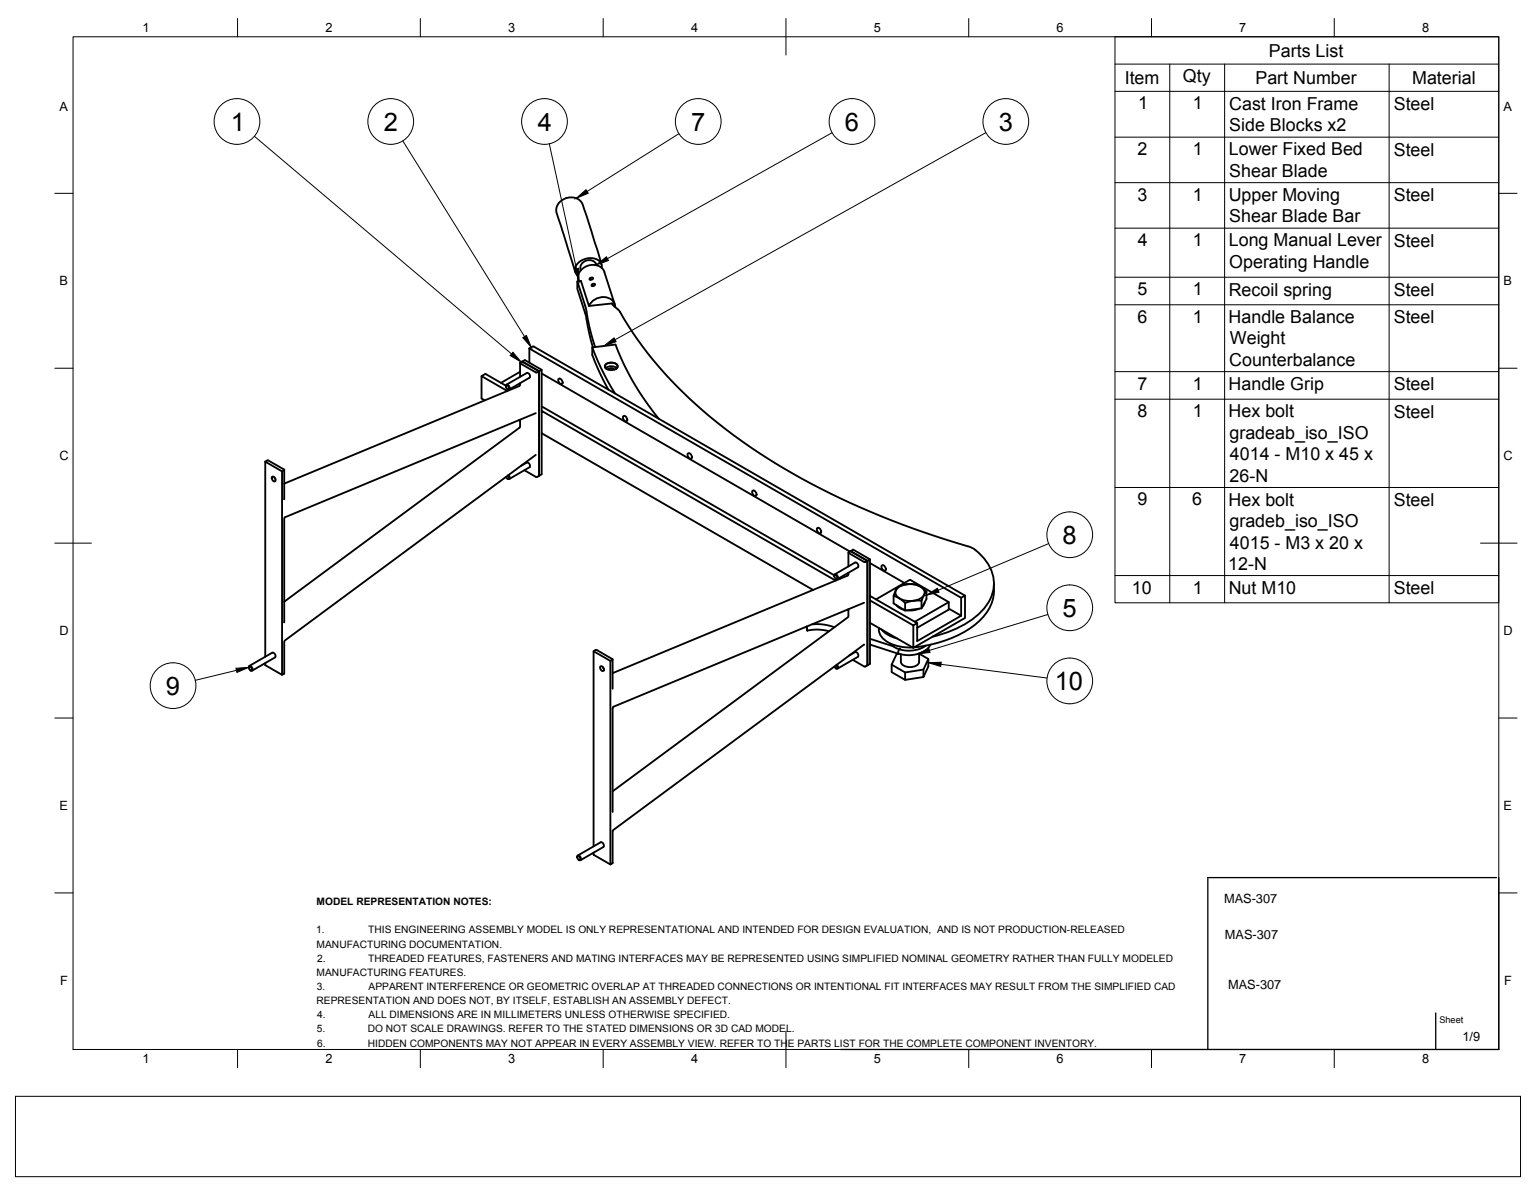
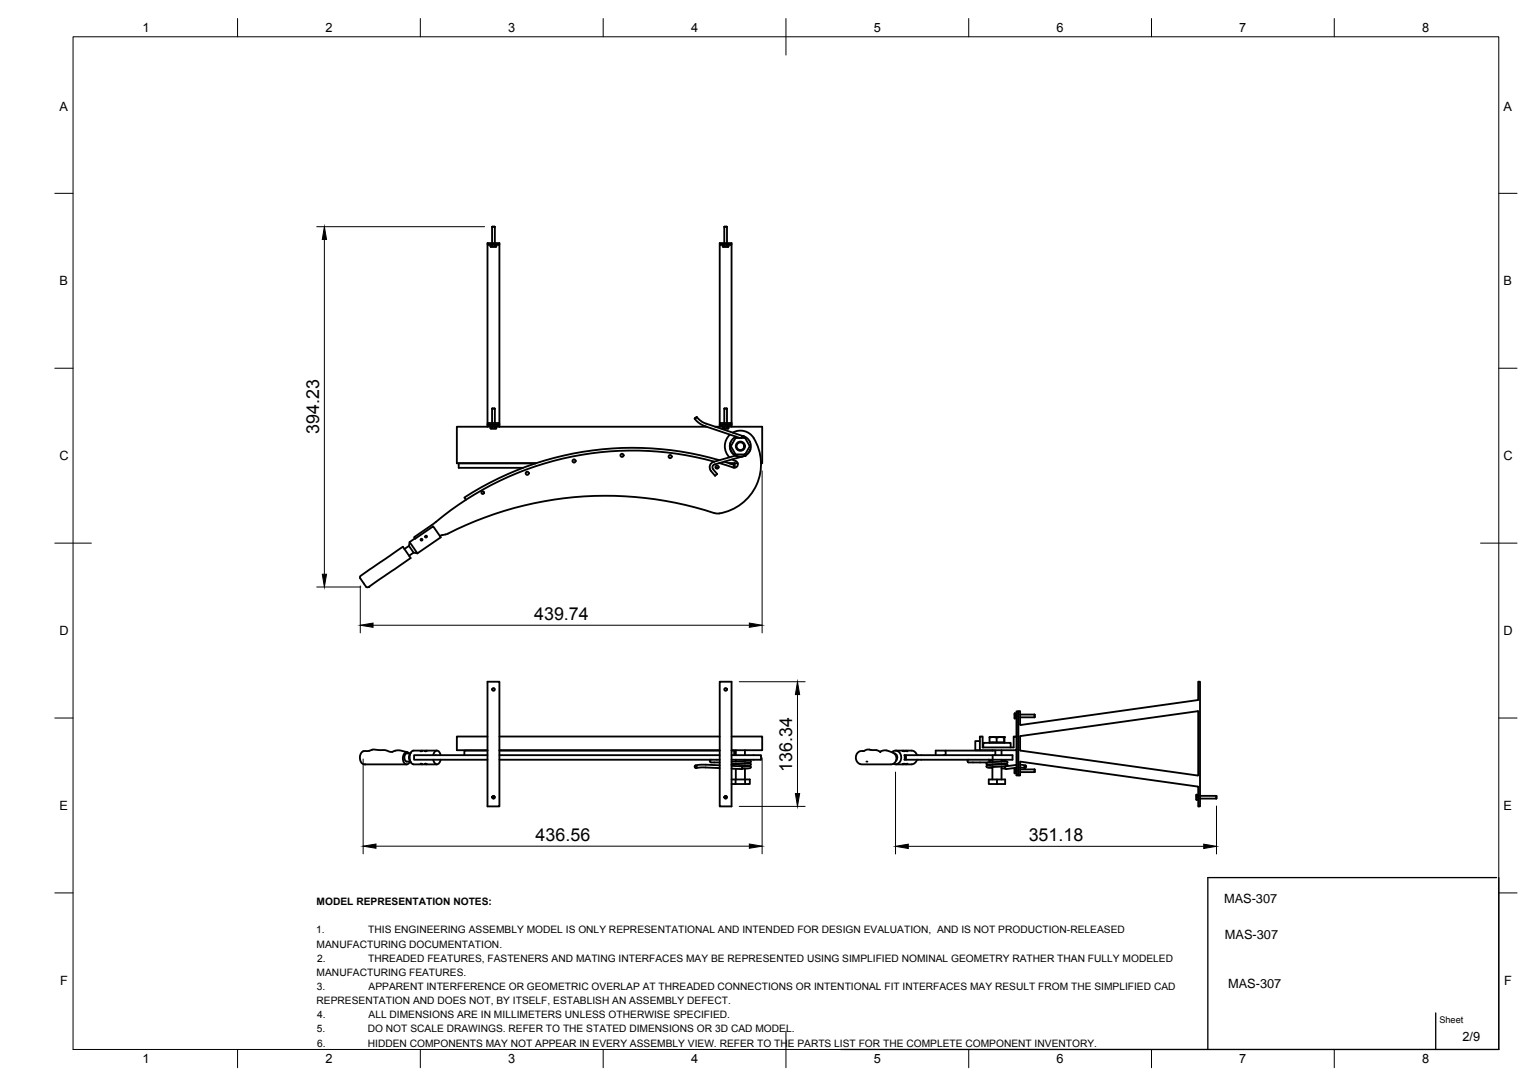
ISO-10303-21;
HEADER;
FILE_DESCRIPTION (('STEP AP214'),
    '1' );
FILE_NAME ('MAS-307',
    '2026-10-06T07:34:29',
    ( '' ),
    ( '' ),
    'SwSTEP 2.0',
    'SolidWorks 2025',
    '' );
FILE_SCHEMA (( 'AUTOMOTIVE_DESIGN' ));
ENDSEC;

DATA;
#1 = ORIENTED_EDGE ( 'NONE', *, *, #36, .T. ) ;
#2 = DIRECTION ( 'NONE',  ( 0.000000000000000000, 0.000000000000000000, -1.000000000000000000 ) ) ;
#3 = CIRCLE ( 'NONE', #12613, 8.000000000000028422 ) ;
#4 = CARTESIAN_POINT ( 'NONE',  ( 177.5000000000000853, 15.47035339324670922, 37.00486596562913633 ) ) ;
#5 = CIRCLE ( 'NONE', #1538, 3.525000000000000355 ) ;
#6 = CARTESIAN_POINT ( 'NONE',  ( -167.5053995445195767, 127.4304153265770907, 2.500000001036336350 ) ) ;
#7 = CARTESIAN_POINT ( 'NONE',  ( -70.00000000000000000, -201.3058001507315566, -41.45141194869120227 ) ) ;
#8 = ORIENTED_EDGE ( 'NONE', *, *, #9613, .T. ) ;
#9 = EDGE_LOOP ( 'NONE', ( #498, #10940, #14960, #5861, #9835 ) ) ;
#10 = CARTESIAN_POINT ( 'NONE',  ( -168.3602667112202766, 125.8948777600411830, -3.002243219525047024 ) ) ;
#11 = CARTESIAN_POINT ( 'NONE',  ( 205.4931693814993139, 33.91842896272902408, -6.501828201457912293 ) ) ;
#12 = ORIENTED_EDGE ( 'NONE', *, *, #8305, .F. ) ;
#13 = DIRECTION ( 'NONE',  ( 0.000000000000000000, 0.1391731009600660485, -0.9902680687415702510 ) ) ;
#14 = LINE ( 'NONE', #12973, #6716 ) ;
#15 = CARTESIAN_POINT ( 'NONE',  ( 66.76535645333922275, 38.79159067395544014, 7.600000000000002309 ) ) ;
#16 = VECTOR ( 'NONE', #3003, 1000.000000000000000 ) ;
#17 = EDGE_CURVE ( 'NONE', #5528, #10245, #15139, .T. ) ;
#18 = MECHANICAL_DESIGN_GEOMETRIC_PRESENTATION_REPRESENTATION (  '', ( #1288 ), #7370 ) ;
#19 = ORIENTED_EDGE ( 'NONE', *, *, #12875, .F. ) ;
#20 = DIRECTION ( 'NONE',  ( -0.000000000000000000, -0.000000000000000000, 1.000000000000000000 ) ) ;
#21 = CARTESIAN_POINT ( 'NONE',  ( 205.4699394944333051, 33.88363592193200446, -7.930995773285529182 ) ) ;
#22 = ORIENTED_EDGE ( 'NONE', *, *, #8785, .F. ) ;
#23 = DIRECTION ( 'NONE',  ( -0.000000000000000000, 1.156482317317871478E-16, -1.000000000000000000 ) ) ;
#24 = CARTESIAN_POINT ( 'NONE',  ( -136.1405586187959784, 108.3975249866138597, 0.000000000000000000 ) ) ;
#25 = CARTESIAN_POINT ( 'NONE',  ( -225.5636091402884915, 143.1065995042388863, -0.5218507872395625746 ) ) ;
#26 = LINE ( 'NONE', #1296, #2230 ) ;
#27 = ORIENTED_EDGE ( 'NONE', *, *, #13841, .F. ) ;
#28 = CARTESIAN_POINT ( 'NONE',  ( -185.2335129678179726, 125.0353967269121966, 9.577123744044223841 ) ) ;
#30 = CARTESIAN_POINT ( 'NONE',  ( 198.8634854004546071, 49.55149448133588663, -6.680369717582868461 ) ) ;
#29 = VECTOR ( 'NONE', #1575, 1000.000000000000000 ) ;
#31 = ORIENTED_EDGE ( 'NONE', *, *, #9479, .F. ) ;
#32 = ORIENTED_EDGE ( 'NONE', *, *, #11983, .F. ) ;
#33 = VECTOR ( 'NONE', #1804, 1000.000000000000000 ) ;
#34 = DIRECTION ( 'NONE',  ( -0.000000000000000000, -0.000000000000000000, 1.000000000000000000 ) ) ;
#35 = LINE ( 'NONE', #4552, #8075 ) ;
#36 = EDGE_CURVE ( 'NONE', #15150, #10379, #8408, .T. ) ;
#37 = DIRECTION ( 'NONE',  ( 0.000000000000000000, 0.000000000000000000, -1.000000000000000000 ) ) ;
#38 = DIRECTION ( 'NONE',  ( 1.000000000000000000, 0.000000000000000000, 0.000000000000000000 ) ) ;
#39 = CARTESIAN_POINT ( 'NONE',  ( -152.4086188282879277, 107.2728346664360259, 84.88378295107887084 ) ) ;
#40 = PRODUCT_RELATED_PRODUCT_CATEGORY ( 'part', '', ( #10548 ) ) ;
#41 = CARTESIAN_POINT ( 'NONE',  ( -150.4086188282879277, 107.2728346664360259, 5.000000000000004441 ) ) ;
#42 = CONICAL_SURFACE ( 'NONE', #4331, 4.499999999999950262, 0.7853981633974450594 ) ;
#43 = DIRECTION ( 'NONE',  ( 0.000000000000000000, 0.000000000000000000, 1.000000000000000000 ) ) ;
#44 = EDGE_CURVE ( 'NONE', #6556, #10266, #3803, .T. ) ;
#45 = CARTESIAN_POINT ( 'NONE',  ( -76.50000000000001421, 15.03993994372673981, 10.05257423913146475 ) ) ;
#46 = FACE_OUTER_BOUND ( 'NONE', #2849, .T. ) ;
#47 = CARTESIAN_POINT ( 'NONE',  ( 70.26535645333922275, 38.79159067395544014, 10.00000000000000178 ) ) ;
#48 = CARTESIAN_POINT ( 'NONE',  ( 177.5000000000000853, 15.03993994372673804, 24.94742576086838781 ) ) ;
#49 = ORIENTED_EDGE ( 'NONE', *, *, #2623, .T. ) ;
#50 = VERTEX_POINT ( 'NONE', #13007 ) ;
#51 = DIRECTION ( 'NONE',  ( 1.000000000000000000, 0.000000000000000000, 0.000000000000000000 ) ) ;
#52 = CARTESIAN_POINT ( 'NONE',  ( -36.49899788034579018, 48.72489408690345414, 5.000000000000000000 ) ) ;
#53 = PLANE ( 'NONE',  #11171 ) ;
#54 = FACE_OUTER_BOUND ( 'NONE', #8334, .T. ) ;
#55 = CARTESIAN_POINT ( 'NONE',  ( -76.50000000000001421, 19.53993994372674692, -17.50000000000002487 ) ) ;
#56 = TOROIDAL_SURFACE ( 'NONE', #1821, 4.799128011492294732, 1.499999999999997113 ) ;
#57 = DIRECTION ( 'NONE',  ( 1.000000000000000000, 0.000000000000000000, 0.000000000000000000 ) ) ;
#58 = FACE_OUTER_BOUND ( 'NONE', #1129, .T. ) ;
#59 = EDGE_CURVE ( 'NONE', #163, #6601, #13932, .T. ) ;
#60 = EDGE_CURVE ( 'NONE', #13786, #6568, #5831, .T. ) ;
#61 = VERTEX_POINT ( 'NONE', #1883 ) ;
#62 = AXIS2_PLACEMENT_3D ( 'NONE', #15140, #11528, #6573 ) ;
#63 = ORIENTED_EDGE ( 'NONE', *, *, #11844, .T. ) ;
#64 = CARTESIAN_POINT ( 'NONE',  ( 207.1592428330643827, 35.64176030267155681, -3.375779224823745928 ) ) ;
#65 = LINE ( 'NONE', #4977, #10142 ) ;
#66 = ORIENTED_EDGE ( 'NONE', *, *, #14903, .T. ) ;
#67 = VECTOR ( 'NONE', #9001, 1000.000000000000000 ) ;
#68 = CARTESIAN_POINT ( 'NONE',  ( -223.5763732829059904, 146.6670444861485976, 6.843617190574383891 ) ) ;
#69 = EDGE_LOOP ( 'NONE', ( #4641, #9788 ) ) ;
#70 = DIRECTION ( 'NONE',  ( -3.965082230804130220E-16, -0.000000000000000000, -1.000000000000000000 ) ) ;
#71 = CARTESIAN_POINT ( 'NONE',  ( 198.4684236769687686, 29.09143143995051872, -2.316743362709667409 ) ) ;
#72 = EDGE_CURVE ( 'NONE', #11235, #14746, #6724, .T. ) ;
#74 = ORIENTED_EDGE ( 'NONE', *, *, #9272, .F. ) ;
#73 = AXIS2_PLACEMENT_3D ( 'NONE', #11589, #11673, #2027 ) ;
#75 = FACE_OUTER_BOUND ( 'NONE', #2731, .T. ) ;
#76 = CARTESIAN_POINT ( 'NONE',  ( 70.26535645333922275, 38.79159067395544014, 7.600000000000002309 ) ) ;
#77 = LINE ( 'NONE', #10922, #4868 ) ;
#78 = VECTOR ( 'NONE', #416, 1000.000000000000000 ) ;
#79 = ORIENTED_EDGE ( 'NONE', *, *, #3059, .T. ) ;
#80 = CIRCLE ( 'NONE', #13699, 3.525000000000000355 ) ;
#81 = CARTESIAN_POINT ( 'NONE',  ( -110.0000000000000426, 59.53993994372674337, 10.00000000000000178 ) ) ;
#82 = DIRECTION ( 'NONE',  ( -0.000000000000000000, -0.000000000000000000, 1.000000000000000000 ) ) ;
#83 = ADVANCED_FACE ( 'NONE', ( #687 ), #5531, .F. ) ;
#84 = DIRECTION ( 'NONE',  ( 1.000000000000000000, 0.000000000000000000, 0.000000000000000000 ) ) ;
#85 = VERTEX_POINT ( 'NONE', #2360 ) ;
#86 = EDGE_LOOP ( 'NONE', ( #3348, #2604, #2165, #14498 ) ) ;
#87 = CARTESIAN_POINT ( 'NONE',  ( -207.0700983879231387, 149.0508413170868209, -0.4547266291960758156 ) ) ;
#88 = CARTESIAN_POINT ( 'NONE',  ( 198.7876695280922661, 49.53587328158837977, -8.249370650301745655 ) ) ;
#89 = ORIENTED_EDGE ( 'NONE', *, *, #715, .T. ) ;
#90 = LINE ( 'NONE', #10937, #11841 ) ;
#91 = FACE_OUTER_BOUND ( 'NONE', #15309, .T. ) ;
#92 = CARTESIAN_POINT ( 'NONE',  ( 178.0000000000000853, 15.03993994372673981, -3.075184203610571654 ) ) ;
#93 = ORIENTED_EDGE ( 'NONE', *, *, #2529, .F. ) ;
#94 = AXIS2_PLACEMENT_3D ( 'NONE', #7418, #12210, #6221 ) ;
#95 = CARTESIAN_POINT ( 'NONE',  ( 201.7406124912899941, 52.65652330452660834, -2.244206067705167396 ) ) ;
#96 = ORIENTED_EDGE ( 'NONE', *, *, #2656, .T. ) ;
#97 = CARTESIAN_POINT ( 'NONE',  ( -34.79899788034579444, 48.72489408690345414, 10.00000000000000178 ) ) ;
#98 = CARTESIAN_POINT ( 'NONE',  ( 175.9483885134608272, -181.3058001507315566, -51.45141194869120227 ) ) ;
#99 = CARTESIAN_POINT ( 'NONE',  ( -218.1518098834511648, 139.2461763302102327, 3.478895870929506362 ) ) ;
#100 = DIRECTION ( 'NONE',  ( -1.000000000000000000, 0.000000000000000000, 0.000000000000000000 ) ) ;
#101 = VERTEX_POINT ( 'NONE', #4890 ) ;
#102 = CARTESIAN_POINT ( 'NONE',  ( -182.6699909761611877, 123.4132960977408970, 9.577123744044220288 ) ) ;
#103 = CARTESIAN_POINT ( 'NONE',  ( 202.3883256910358739, 32.65987148549056229, -8.116337980372584582 ) ) ;
#104 = ORIENTED_EDGE ( 'NONE', *, *, #13012, .T. ) ;
#105 = ORIENTED_EDGE ( 'NONE', *, *, #5952, .T. ) ;
#106 = CYLINDRICAL_SURFACE ( 'NONE', #2526, 3.752352628381527833 ) ;
#107 = LINE ( 'NONE', #4949, #8591 ) ;
#108 = VECTOR ( 'NONE', #10524, 1000.000000000000000 ) ;
#109 = DIRECTION ( 'NONE',  ( -0.000000000000000000, -0.000000000000000000, 1.000000000000000000 ) ) ;
#110 = CARTESIAN_POINT ( 'NONE',  ( 5.799999999999999822, -4.618802153517037823, -7.999999999999979572 ) ) ;
#111 = ADVANCED_FACE ( 'NONE', ( #1394 ), #10899, .F. ) ;
#112 = CARTESIAN_POINT ( 'NONE',  ( -225.3482675701515348, 143.4924177300907502, -0.7821592797845021705 ) ) ;
#113 = DIRECTION ( 'NONE',  ( 1.000000000000000000, 0.000000000000000000, 0.000000000000000000 ) ) ;
#114 = CARTESIAN_POINT ( 'NONE',  ( -35.99999999999995026, 62.13993994372673768, 18.50000000000140332 ) ) ;
#115 = AXIS2_PLACEMENT_3D ( 'NONE', #5696, #3243, #10590 ) ;
#116 = CARTESIAN_POINT ( 'NONE',  ( -108.0000000000000568, 64.53993994372673626, 20.00000000000000355 ) ) ;
#117 = DIRECTION ( 'NONE',  ( 0.000000000000000000, 0.000000000000000000, 1.000000000000000000 ) ) ;
#118 = ORIENTED_EDGE ( 'NONE', *, *, #6762, .T. ) ;
#119 = CARTESIAN_POINT ( 'NONE',  ( 114.0000000000000568, 64.53993994372673626, 11.50000000000034817 ) ) ;
#120 = ADVANCED_FACE ( 'NONE', ( #7198 ), #13161, .F. ) ;
#121 = ORIENTED_EDGE ( 'NONE', *, *, #6164, .F. ) ;
#122 = DIRECTION ( 'NONE',  ( 1.000000000000000000, 0.000000000000000000, 0.000000000000000000 ) ) ;
#123 = DIRECTION ( 'NONE',  ( -0.9741547192086867923, 0.2258817899775114602, 0.000000000000000000 ) ) ;
#124 = FACE_OUTER_BOUND ( 'NONE', #1519, .T. ) ;
#125 = LINE ( 'NONE', #13401, #6173 ) ;
#126 = CARTESIAN_POINT ( 'NONE',  ( 185.1062858801516882, 25.86394065090268057, 18.00000000000000355 ) ) ;
#127 = CARTESIAN_POINT ( 'NONE',  ( 0.000000000000000000, -2.381569860407207084, -1.374999999999997113 ) ) ;
#128 = DIRECTION ( 'NONE',  ( 0.000000000000000000, 0.000000000000000000, -1.000000000000000000 ) ) ;
#129 = AXIS2_PLACEMENT_3D ( 'NONE', #758, #2991, #9229 ) ;
#130 = EDGE_LOOP ( 'NONE', ( #9688, #11393, #15136, #3970 ) ) ;
#131 = ORIENTED_EDGE ( 'NONE', *, *, #13724, .F. ) ;
#132 = CARTESIAN_POINT ( 'NONE',  ( 202.9578473199472057, 32.84482942423175444, -9.656098271102047548 ) ) ;
#133 = CARTESIAN_POINT ( 'NONE',  ( -221.9693044472552117, 149.5463605724702916, 7.947916423171728084 ) ) ;
#134 = ORIENTED_EDGE ( 'NONE', *, *, #1310, .F. ) ;
#135 = ADVANCED_FACE ( 'NONE', ( #124, #11996 ), #53, .F. ) ;
#136 = CARTESIAN_POINT ( 'NONE',  ( -222.7380986314676363, 148.1689451111236906, 7.733218891984481758 ) ) ;
#137 = EDGE_CURVE ( 'NONE', #9526, #14472, #1038, .T. ) ;
#138 = VERTEX_POINT ( 'NONE', #10733 ) ;
#139 = CARTESIAN_POINT ( 'NONE',  ( 164.0000000000000568, 64.53993994372673626, 16.70000000000000995 ) ) ;
#140 = AXIS2_PLACEMENT_3D ( 'NONE', #4727, #9874, #2603 ) ;
#141 = CARTESIAN_POINT ( 'NONE',  ( 177.5000000000000853, -179.3058001507315566, -51.45141194869120227 ) ) ;
#142 = CIRCLE ( 'NONE', #13010, 4.499999999999950262 ) ;
#143 = ORIENTED_EDGE ( 'NONE', *, *, #13656, .T. ) ;
#144 = CARTESIAN_POINT ( 'NONE',  ( 114.0000000000000426, 15.53993994372673981, 7.305634244248866343E-16 ) ) ;
#145 = DIRECTION ( 'NONE',  ( -5.518327896226365911E-17, 0.9902680687415714722, -0.1391731009600582769 ) ) ;
#146 = B_SPLINE_CURVE_WITH_KNOTS ( 'NONE', 3,
 ( #5136, #531, #1653, #11218, #9963, #14979, #8698, #12464, #14906, #1729, #5371, #4019, #13643, #371, #7438, #2772, #5212, #6490, #11287, #14749, #7674, #6569, #448, #13727, #10034, #10112, #10189, #12233, #8933, #1411, #2930, #11372, #4170, #6248, #1492, #211, #11061, #2692, #5059, #9884, #14674, #3874, #685, #1881, #15369, #849, #13889, #9240 ),
 .UNSPECIFIED., .F., .F.,
 ( 4, 2, 2, 2, 2, 2, 2, 2, 2, 2, 2, 2, 2, 2, 2, 2, 2, 2, 2, 2, 2, 2, 2, 4 ),
 ( 0.02192817935270313656, 0.02330785662426448565, 0.02399769526004516540, 0.02468753389582584862, 0.02606721116738722893, 0.02675704980316793297, 0.02744688843894863700, 0.02882656571051007630, 0.02951640434629079768, 0.03020624298207151559, 0.03158592025363299305, 0.03227575888941371096, 0.03296559752519442887, 0.03365543616097514679, 0.03434527479675586470, 0.03572495206831733522, 0.03641479070409808783, 0.03710462933987884043, 0.03779446797565959304, 0.03848430661144034565, 0.03986398388300183004, 0.04124366115456330750, 0.04262333842612478496, 0.04400301569768626936 ),
 .UNSPECIFIED. ) ;
#147 = PLANE ( 'NONE',  #811 ) ;
#148 = EDGE_LOOP ( 'NONE', ( #966, #9881, #15338, #13043 ) ) ;
#149 = ORIENTED_EDGE ( 'NONE', *, *, #15360, .T. ) ;
#150 = CARTESIAN_POINT ( 'NONE',  ( 190.5000000000000568, -181.3058001507315566, 84.88378295107885663 ) ) ;
#151 = ORIENTED_EDGE ( 'NONE', *, *, #11944, .F. ) ;
#152 = FACE_OUTER_BOUND ( 'NONE', #9575, .T. ) ;
#153 = CARTESIAN_POINT ( 'NONE',  ( -152.0435700508773209, 108.0561044943065951, -4.829560219627783368 ) ) ;
#154 = ORIENTED_EDGE ( 'NONE', *, *, #12875, .T. ) ;
#155 = ORIENTED_EDGE ( 'NONE', *, *, #7793, .T. ) ;
#156 = CARTESIAN_POINT ( 'NONE',  ( -179.9223906590855222, 134.3711564447467310, 1.515441477536284554 ) ) ;
#157 = CARTESIAN_POINT ( 'NONE',  ( -223.6137413416247739, 142.0138547493179146, 2.263321283727593336 ) ) ;
#158 = VERTEX_POINT ( 'NONE', #7269 ) ;
#159 = CIRCLE ( 'NONE', #9018, 4.499999999999950262 ) ;
#160 = DIRECTION ( 'NONE',  ( 0.000000000000000000, 0.9902680687415712502, 0.1391731009600584990 ) ) ;
#161 = DIRECTION ( 'NONE',  ( 0.000000000000000000, 0.000000000000000000, -1.000000000000000000 ) ) ;
#162 = DIRECTION ( 'NONE',  ( 8.659560562354932858E-17, 0.7071067811865474617, -0.7071067811865474617 ) ) ;
#163 = VERTEX_POINT ( 'NONE', #8301 ) ;
#164 = EDGE_CURVE ( 'NONE', #1358, #7203, #12629, .T. ) ;
#165 = LINE ( 'NONE', #5013, #3777 ) ;
#166 = CARTESIAN_POINT ( 'NONE',  ( 198.3913412372077687, 29.09831693401786268, -0.7477385443502184703 ) ) ;
#167 = ORIENTED_EDGE ( 'NONE', *, *, #13377, .T. ) ;
#168 = CARTESIAN_POINT ( 'NONE',  ( -64.00000000000002842, 15.53993994372673981, -3.075184203610571654 ) ) ;
#169 = AXIS2_PLACEMENT_3D ( 'NONE', #9896, #5224, #1587 ) ;
#170 = CARTESIAN_POINT ( 'NONE',  ( -183.7136537759689929, 127.7093858820786068, -5.230826428279597096 ) ) ;
#171 = CARTESIAN_POINT ( 'NONE',  ( -63.50000000000002842, 15.03993994372673981, -3.075184203610571654 ) ) ;
#172 = ORIENTED_EDGE ( 'NONE', *, *, #9722, .T. ) ;
#173 = CARTESIAN_POINT ( 'NONE',  ( -197.4591130885309553, 135.0981391493542105, 10.16010209732750802 ) ) ;
#174 = CARTESIAN_POINT ( 'NONE',  ( 207.1690005588685040, 46.08364065960329725, 0.3832845883476674320 ) ) ;
#175 = ORIENTED_EDGE ( 'NONE', *, *, #1719, .F. ) ;
#176 = VERTEX_POINT ( 'NONE', #14424 ) ;
#177 = AXIS2_PLACEMENT_3D ( 'NONE', #9070, #13874, #12756 ) ;
#178 = CARTESIAN_POINT ( 'NONE',  ( -85.99999999999994316, 64.51493994372674479, 18.50000000000175149 ) ) ;
#179 = DIRECTION ( 'NONE',  ( 0.000000000000000000, 0.000000000000000000, 1.000000000000000000 ) ) ;
#180 =( GEOMETRIC_REPRESENTATION_CONTEXT ( 3 ) GLOBAL_UNCERTAINTY_ASSIGNED_CONTEXT ( ( #8186 ) ) GLOBAL_UNIT_ASSIGNED_CONTEXT ( ( #3150, #4481, #1954 ) ) REPRESENTATION_CONTEXT ( 'NONE', 'WORKASPACE' ) );
#181 = CARTESIAN_POINT ( 'NONE',  ( 200.1062858801516597, 40.86394065090267702, 12.00000000000001066 ) ) ;
#182 = TOROIDAL_SURFACE ( 'NONE', #1206, 1.000000000000000000, 0.5000000000000000000 ) ;
#183 = DIRECTION ( 'NONE',  ( 1.000000000000000000, 0.000000000000000000, 0.000000000000000000 ) ) ;
#184 = DIRECTION ( 'NONE',  ( -0.000000000000000000, -0.000000000000000000, 1.000000000000000000 ) ) ;
#185 = AXIS2_PLACEMENT_3D ( 'NONE', #1249, #10903, #14351 ) ;
#186 = DIRECTION ( 'NONE',  ( 0.000000000000000000, 0.000000000000000000, 1.000000000000000000 ) ) ;
#187 = DIRECTION ( 'NONE',  ( 0.000000000000000000, 0.000000000000000000, 1.000000000000000000 ) ) ;
#188 = PRODUCT_DEFINITION_FORMATION_WITH_SPECIFIED_SOURCE ( 'ANY', '', #10425, .NOT_KNOWN. ) ;
#189 = ORIENTED_EDGE ( 'NONE', *, *, #8600, .F. ) ;
#190 = ADVANCED_FACE ( 'NONE', ( #12144 ), #4855, .T. ) ;
#191 = AXIS2_PLACEMENT_3D ( 'NONE', #8581, #13373, #8730 ) ;
#192 = ORIENTED_EDGE ( 'NONE', *, *, #11037, .F. ) ;
#193 = DIRECTION ( 'NONE',  ( 0.000000000000000000, 0.000000000000000000, -1.000000000000000000 ) ) ;
#194 = LINE ( 'NONE', #8457, #6371 ) ;
#195 = DIRECTION ( 'NONE',  ( 1.000000000000000000, 0.000000000000000000, -0.000000000000000000 ) ) ;
#196 = DIRECTION ( 'NONE',  ( 0.000000000000000000, 0.000000000000000000, 1.000000000000000000 ) ) ;
#197 = DIRECTION ( 'NONE',  ( 1.000000000000000000, 0.000000000000000000, 0.000000000000000000 ) ) ;
#198 = DIRECTION ( 'NONE',  ( 0.000000000000000000, 0.000000000000000000, 1.000000000000000000 ) ) ;
#199 = CARTESIAN_POINT ( 'NONE',  ( -185.2055264765504887, 137.3096093875189467, 2.500000000000000000 ) ) ;
#200 = VECTOR ( 'NONE', #3620, 1000.000000000000000 ) ;
#201 = EDGE_LOOP ( 'NONE', ( #1693, #11095, #14591, #7867 ) ) ;
#202 = AXIS2_PLACEMENT_3D ( 'NONE', #6427, #5227, #1671 ) ;
#203 = EDGE_CURVE ( 'NONE', #12014, #13507, #9648, .T. ) ;
#204 = DIRECTION ( 'NONE',  ( 1.000000000000000000, 0.000000000000000000, 0.000000000000000000 ) ) ;
#205 = CARTESIAN_POINT ( 'NONE',  ( 205.4339596421060889, 33.86846485884471747, -4.932823326473320336 ) ) ;
#206 = CARTESIAN_POINT ( 'NONE',  ( -224.5476011597490356, 144.9269372877251669, 3.604463283145519448 ) ) ;
#207 = VERTEX_POINT ( 'NONE', #5995 ) ;
#208 = CIRCLE ( 'NONE', #2252, 1.499999999999996891 ) ;
#209 = CARTESIAN_POINT ( 'NONE',  ( -222.3356595723642215, 144.5667354790973604, 8.419022500423421818 ) ) ;
#210 = EDGE_LOOP ( 'NONE', ( #10445, #12034, #11284, #6545 ) ) ;
#211 = CARTESIAN_POINT ( 'NONE',  ( -172.9645346626803359, 118.3395572346633173, -3.768257758897336274 ) ) ;
#212 = CARTESIAN_POINT ( 'NONE',  ( 192.9105869384611935, 31.39693960586098598, -5.567602151433582058 ) ) ;
#213 = CIRCLE ( 'NONE', #730, 1.000000000000000888 ) ;
#214 = VECTOR ( 'NONE', #12787, 1000.000000000000227 ) ;
#215 = ORIENTED_EDGE ( 'NONE', *, *, #12661, .T. ) ;
#216 = CARTESIAN_POINT ( 'NONE',  ( -61.94838851346079167, -178.8058001507315566, 52.69066787724494816 ) ) ;
#217 = CARTESIAN_POINT ( 'NONE',  ( -76.00000000000001421, 15.53993994372674159, 9.617930870223352358 ) ) ;
#218 = EDGE_CURVE ( 'NONE', #11968, #7924, #4346, .T. ) ;
#219 = AXIS2_PLACEMENT_3D ( 'NONE', #7961, #12749, #6770 ) ;
#220 = DIRECTION ( 'NONE',  ( -0.000000000000000000, 1.486905836551548832E-16, -1.000000000000000000 ) ) ;
#221 = ORIENTED_EDGE ( 'NONE', *, *, #12224, .F. ) ;
#222 =( GEOMETRIC_REPRESENTATION_CONTEXT ( 3 ) GLOBAL_UNCERTAINTY_ASSIGNED_CONTEXT ( ( #10529 ) ) GLOBAL_UNIT_ASSIGNED_CONTEXT ( ( #15547, #7222, #9271 ) ) REPRESENTATION_CONTEXT ( 'NONE', 'WORKASPACE' ) );
#223 = AXIS2_PLACEMENT_3D ( 'NONE', #7936, #9115, #2067 ) ;
#224 = PRODUCT_RELATED_PRODUCT_CATEGORY ( 'part', '', ( #9174 ) ) ;
#225 = EDGE_CURVE ( 'NONE', #176, #7789, #1243, .T. ) ;
#226 = DIRECTION ( 'NONE',  ( 1.156482317317871725E-16, 1.156482317317871725E-16, -1.000000000000000000 ) ) ;
#227 = VERTEX_POINT ( 'NONE', #12067 ) ;
#228 = LINE ( 'NONE', #150, #2384 ) ;
#229 = EDGE_CURVE ( 'NONE', #11059, #5257, #8156, .T. ) ;
#230 = EDGE_LOOP ( 'NONE', ( #7966, #6489 ) ) ;
#231 = DIRECTION ( 'NONE',  ( 0.9296197478520974444, 0.3660421972118351741, -0.04266420354037655377 ) ) ;
#232 = DIRECTION ( 'NONE',  ( -0.000000000000000000, 1.000000000000000000, 1.156482317317871725E-16 ) ) ;
#233 = AXIS2_PLACEMENT_3D ( 'NONE', #7331, #6137, #10957 ) ;
#234 = VERTEX_POINT ( 'NONE', #13400 ) ;
#235 = VERTEX_POINT ( 'NONE', #8458 ) ;
#236 = LINE ( 'NONE', #6353, #3489 ) ;
#237 = CARTESIAN_POINT ( 'NONE',  ( 207.1194509196011495, 46.14302886020001182, -1.185720282267065828 ) ) ;
#238 = VECTOR ( 'NONE', #1875, 1000.000000000000000 ) ;
#239 = ORIENTED_EDGE ( 'NONE', *, *, #3705, .T. ) ;
#240 = DIRECTION ( 'NONE',  ( 0.000000000000000000, -1.000000000000000000, 0.000000000000000000 ) ) ;
#241 = CARTESIAN_POINT ( 'NONE',  ( 190.0000000000000568, -179.3058001507315282, -29.88378295107906268 ) ) ;
#242 = FACE_OUTER_BOUND ( 'NONE', #9642, .T. ) ;
#243 = MANIFOLD_SOLID_BREP ( 'HeadFillet', #9878 ) ;
#244 = EDGE_CURVE ( 'NONE', #1879, #4614, #5269, .T. ) ;
#245 = EDGE_CURVE ( 'NONE', #3324, #6496, #6158, .T. ) ;
#246 = AXIS2_PLACEMENT_3D ( 'NONE', #10758, #10919, #3716 ) ;
#247 = CIRCLE ( 'NONE', #14631, 0.5000000000000069944 ) ;
#248 =( LENGTH_UNIT ( ) NAMED_UNIT ( * ) SI_UNIT ( .MILLI., .METRE. ) );
#249 = CARTESIAN_POINT ( 'NONE',  ( 194.7047954745769687, 33.92018974228710704, -0.9908858387024377379 ) ) ;
#250 = ORIENTED_EDGE ( 'NONE', *, *, #12118, .T. ) ;
#251 = DIRECTION ( 'NONE',  ( 0.000000000000000000, 6.938893903907227145E-17, -1.000000000000000000 ) ) ;
#252 = CYLINDRICAL_SURFACE ( 'NONE', #13481, 1.700000000000007061 ) ;
#253 = EDGE_CURVE ( 'NONE', #2275, #9404, #10915, .T. ) ;
#254 = CARTESIAN_POINT ( 'NONE',  ( -176.4863952559862526, 117.0241230567913959, -0.6469977504890583875 ) ) ;
#255 = DIRECTION ( 'NONE',  ( -0.000000000000000000, -0.000000000000000000, 1.000000000000000000 ) ) ;
#256 = VERTEX_POINT ( 'NONE', #7495 ) ;
#257 = CARTESIAN_POINT ( 'NONE',  ( -171.9895241055258168, 125.0924944214600885, 9.516496325551347724 ) ) ;
#258 = CARTESIAN_POINT ( 'NONE',  ( 202.9147226314038051, 48.88641379461363101, -0.9068510277452211943 ) ) ;
#259 = VERTEX_POINT ( 'NONE', #512 ) ;
#260 = EDGE_LOOP ( 'NONE', ( #8120, #14477, #13087, #8621 ) ) ;
#261 = VECTOR ( 'NONE', #6975, 1000.000000000000000 ) ;
#262 = ADVANCED_FACE ( 'NONE', ( #11203, #355 ), #1639, .F. ) ;
#263 = CARTESIAN_POINT ( 'NONE',  ( 14.00000000000004086, 64.53993994372673626, 15.00000000000104983 ) ) ;
#264 = CARTESIAN_POINT ( 'NONE',  ( 0.000000000000000000, 17.53993994372673981, 8.693413025030312018E-16 ) ) ;
#265 = AXIS2_PLACEMENT_3D ( 'NONE', #2568, #9839, #9679 ) ;
#266 = DIRECTION ( 'NONE',  ( -0.000000000000000000, -0.000000000000000000, 1.000000000000000000 ) ) ;
#267 = DIRECTION ( 'NONE',  ( 0.000000000000000000, -1.000000000000000000, -1.156482317317871478E-16 ) ) ;
#268 = AXIS2_PLACEMENT_3D ( 'NONE', #5608, #7835, #11451 ) ;
#269 = MANIFOLD_SOLID_BREP ( 'Move Face1', #9158 ) ;
#270 = LINE ( 'NONE', #1701, #14484 ) ;
#271 = CARTESIAN_POINT ( 'NONE',  ( -218.6464950597879238, 155.4996951832063701, 5.432615396193927637 ) ) ;
#272 = CARTESIAN_POINT ( 'NONE',  ( 14.00000000000004086, 62.13993994372673768, 15.00000000000104983 ) ) ;
#273 = VECTOR ( 'NONE', #10509, 1000.000000000000000 ) ;
#274 = FACE_BOUND ( 'NONE', #5485, .T. ) ;
#275 = ORIENTED_EDGE ( 'NONE', *, *, #10508, .T. ) ;
#276 = CARTESIAN_POINT ( 'NONE',  ( 215.1062858801516882, 55.86394065090267702, 13.00000000000000178 ) ) ;
#277 = ORIENTED_EDGE ( 'NONE', *, *, #6163, .F. ) ;
#278 = EDGE_CURVE ( 'NONE', #319, #8130, #1801, .T. ) ;
#279 = ORIENTED_EDGE ( 'NONE', *, *, #13409, .F. ) ;
#280 = DIRECTION ( 'NONE',  ( 0.000000000000000000, 0.000000000000000000, 1.000000000000000000 ) ) ;
#281 = DIRECTION ( 'NONE',  ( -0.9741547192086869034, 0.2258817899775114879, 0.000000000000000000 ) ) ;
#282 = CARTESIAN_POINT ( 'NONE',  ( 0.7145311798163189732, 4.618802153516981868, 8.000000000000007105 ) ) ;
#283 = CARTESIAN_POINT ( 'NONE',  ( -64.00000000000002842, -179.3058001507315566, 52.76585208085545275 ) ) ;
#284 = CARTESIAN_POINT ( 'NONE',  ( 71.96535645333923981, 38.79159067395544014, 0.000000000000000000 ) ) ;
#285 = DIRECTION ( 'NONE',  ( 1.000000000000000000, -2.751328491981765035E-32, 3.965082230804130220E-16 ) ) ;
#286 = AXIS2_PLACEMENT_3D ( 'NONE', #9137, #2973, #11498 ) ;
#287 = FACE_OUTER_BOUND ( 'NONE', #14918, .T. ) ;
#288 = CARTESIAN_POINT ( 'NONE',  ( -167.5097532647548633, 127.4226149533560175, 3.478855110549762042 ) ) ;
#289 = AXIS2_PLACEMENT_3D ( 'NONE', #7420, #5036, #8676 ) ;
#290 = ORIENTED_EDGE ( 'NONE', *, *, #8264, .F. ) ;
#291 = CARTESIAN_POINT ( 'NONE',  ( 191.3844089520862894, 42.02011290432638901, -3.056456915890917170 ) ) ;
#292 = CARTESIAN_POINT ( 'NONE',  ( -221.1247960154559280, 151.0594299935001743, 7.622044586438916802 ) ) ;
#293 = ORIENTED_EDGE ( 'NONE', *, *, #8057, .F. ) ;
#294 = CARTESIAN_POINT ( 'NONE',  ( -220.5689849208904150, 152.0552528170083519, 9.261189829759533865 ) ) ;
#295 = VERTEX_POINT ( 'NONE', #2676 ) ;
#296 = LINE ( 'NONE', #14821, #5534 ) ;
#297 = VECTOR ( 'NONE', #7988, 1000.000000000000000 ) ;
#298 = CARTESIAN_POINT ( 'NONE',  ( 204.3096479244403554, 51.57035008254927533, -0.9325724660367167296 ) ) ;
#299 = VERTEX_POINT ( 'NONE', #8683 ) ;
#300 = DIRECTION ( 'NONE',  ( 0.000000000000000000, 1.000000000000000000, 0.000000000000000000 ) ) ;
#301 = DIRECTION ( 'NONE',  ( -0.000000000000000000, 6.938893903907222067E-15, -1.000000000000000000 ) ) ;
#302 = DIRECTION ( 'NONE',  ( 1.000000000000000000, 0.000000000000000000, 0.000000000000000000 ) ) ;
#303 = ORIENTED_EDGE ( 'NONE', *, *, #14000, .F. ) ;
#304 = B_SPLINE_CURVE_WITH_KNOTS ( 'NONE', 3,
 ( #12178, #157, #5002, #3249, #8007 ),
 .UNSPECIFIED., .F., .F.,
 ( 4, 1, 4 ),
 ( 2.671544684753287039E-05, 0.0004182544953931666577, 0.0008097935439387997673 ),
 .UNSPECIFIED. ) ;
#305 = APPLICATION_PROTOCOL_DEFINITION ( 'draft international standard', 'automotive_design', 1998, #4533 ) ;
#306 = ORIENTED_EDGE ( 'NONE', *, *, #7823, .F. ) ;
#307 =( NAMED_UNIT ( * ) SI_UNIT ( $, .STERADIAN. ) SOLID_ANGLE_UNIT ( ) );
#308 = CARTESIAN_POINT ( 'NONE',  ( 177.5000000000000853, 17.53993994372673271, 52.49999999999997868 ) ) ;
#309 = EDGE_LOOP ( 'NONE', ( #6645, #5526, #11534, #9026 ) ) ;
#310 = EDGE_CURVE ( 'NONE', #12060, #3478, #2754, .T. ) ;
#311 = CARTESIAN_POINT ( 'NONE',  ( 21.99999999999999289, 0.000000000000000000, 1.219500000000000028 ) ) ;
#312 = COLOUR_RGB ( '', 0.08235294, 0.09019608, 0.10196078) ;
#313 = CARTESIAN_POINT ( 'NONE',  ( 178.0000000000000853, -179.3058001507315566, 84.88378295107887084 ) ) ;
#314 = ORIENTED_EDGE ( 'NONE', *, *, #44, .F. ) ;
#315 = ORIENTED_EDGE ( 'NONE', *, *, #1829, .T. ) ;
#316 = CARTESIAN_POINT ( 'NONE',  ( -214.8715905313398480, 153.8675021612092451, 2.500000000000000000 ) ) ;
#317 = CARTESIAN_POINT ( 'NONE',  ( 207.1167095084715868, 46.15093117762712893, -7.185265714380067337 ) ) ;
#318 = EDGE_CURVE ( 'NONE', #326, #5664, #13476, .T. ) ;
#319 = VERTEX_POINT ( 'NONE', #10023 ) ;
#320 = AXIS2_PLACEMENT_3D ( 'NONE', #10803, #2269, #8291 ) ;
#321 = FACE_BOUND ( 'NONE', #9577, .T. ) ;
#322 = CARTESIAN_POINT ( 'NONE',  ( -64.00000000000002842, -178.8058001507315566, -17.19066787724516843 ) ) ;
#323 = CARTESIAN_POINT ( 'NONE',  ( 184.0000000000000568, -179.3058001507315566, 76.45141194869098911 ) ) ;
#324 = FACE_OUTER_BOUND ( 'NONE', #11938, .T. ) ;
#325 = CARTESIAN_POINT ( 'NONE',  ( 203.1202131991386182, 29.73909689272393564, -6.555651296533415717 ) ) ;
#326 = VERTEX_POINT ( 'NONE', #14806 ) ;
#327 = DIRECTION ( 'NONE',  ( -0.000000000000000000, 1.000000000000000000, 0.000000000000000000 ) ) ;
#328 = CARTESIAN_POINT ( 'NONE',  ( -223.3178949021943538, 142.5860305806809833, -0.6404123112780930605 ) ) ;
#329 = TOROIDAL_SURFACE ( 'NONE', #6419, 4.799128011492294732, 1.499999999999997113 ) ;
#330 = CARTESIAN_POINT ( 'NONE',  ( -207.1238489746795608, 137.1336079999123854, -4.642206099735007641 ) ) ;
#331 = DIRECTION ( 'NONE',  ( 0.000000000000000000, -0.1391731009600591096, 0.9902680687415711391 ) ) ;
#332 = EDGE_LOOP ( 'NONE', ( #12624, #8209, #7735, #9718 ) ) ;
#333 = CARTESIAN_POINT ( 'NONE',  ( -199.4124801547868913, 127.6177204676982910, 1.515400478619089109 ) ) ;
#334 = CARTESIAN_POINT ( 'NONE',  ( 198.9393012728169765, 49.56711568108339350, -5.111368784863990378 ) ) ;
#335 = EDGE_CURVE ( 'NONE', #2939, #10298, #8373, .T. ) ;
#336 = AXIS2_PLACEMENT_3D ( 'NONE', #14411, #13144, #5897 ) ;
#337 = ORIENTED_EDGE ( 'NONE', *, *, #9909, .T. ) ;
#338 = EDGE_CURVE ( 'NONE', #908, #14204, #13896, .T. ) ;
#339 = ORIENTED_EDGE ( 'NONE', *, *, #2372, .F. ) ;
#340 = DIRECTION ( 'NONE',  ( -0.000000000000000000, 1.000000000000000000, -0.000000000000000000 ) ) ;
#341 = CYLINDRICAL_SURFACE ( 'NONE', #1669, 0.5000000000000004441 ) ;
#342 = FACE_OUTER_BOUND ( 'NONE', #1259, .T. ) ;
#343 = MECHANICAL_DESIGN_GEOMETRIC_PRESENTATION_REPRESENTATION (  '', ( #14469 ), #13976 ) ;
#344 = CARTESIAN_POINT ( 'NONE',  ( 70.26535645333922275, 38.79159067395544014, 5.000000000000000000 ) ) ;
#345 = CARTESIAN_POINT ( 'NONE',  ( 190.0000000000001137, -179.3058001507315566, 84.88378295107887084 ) ) ;
#346 = EDGE_CURVE ( 'NONE', #13457, #11923, #1210, .T. ) ;
#347 = CARTESIAN_POINT ( 'NONE',  ( -76.50000000000001421, 15.53993994372673981, -17.50000000000002487 ) ) ;
#348 = DIRECTION ( 'NONE',  ( 0.000000000000000000, 0.000000000000000000, 1.000000000000000000 ) ) ;
#349 = ORIENTED_EDGE ( 'NONE', *, *, #4874, .F. ) ;
#350 = CARTESIAN_POINT ( 'NONE',  ( -70.00000000000000000, 19.53993994372674337, -12.49999999999999467 ) ) ;
#351 = ORIENTED_EDGE ( 'NONE', *, *, #9722, .F. ) ;
#352 = EDGE_LOOP ( 'NONE', ( #9480, #1820, #544, #3677 ) ) ;
#353 = FACE_OUTER_BOUND ( 'NONE', #13566, .T. ) ;
#354 = DIRECTION ( 'NONE',  ( -0.000000000000000000, -0.000000000000000000, 1.000000000000000000 ) ) ;
#355 = FACE_OUTER_BOUND ( 'NONE', #6775, .T. ) ;
#356 = LINE ( 'NONE', #15042, #7156 ) ;
#357 = CYLINDRICAL_SURFACE ( 'NONE', #6736, 1.700000000000001954 ) ;
#358 = CARTESIAN_POINT ( 'NONE',  ( -218.4414990732828699, 155.8669776719573861, 2.805362964459314323 ) ) ;
#359 = CARTESIAN_POINT ( 'NONE',  ( -218.6464950597879238, 155.4996951832063701, 5.432615396193927637 ) ) ;
#360 = ORIENTED_EDGE ( 'NONE', *, *, #11900, .T. ) ;
#361 = AXIS2_PLACEMENT_3D ( 'NONE', #5638, #4281, #10375 ) ;
#362 = EDGE_CURVE ( 'NONE', #3997, #6369, #2486, .T. ) ;
#363 = FACE_OUTER_BOUND ( 'NONE', #2322, .T. ) ;
#364 = EDGE_CURVE ( 'NONE', #10667, #14434, #6613, .T. ) ;
#365 = ADVANCED_FACE ( 'NONE', ( #3595 ), #14635, .F. ) ;
#366 = CARTESIAN_POINT ( 'NONE',  ( 194.7957337413261030, 33.86335648926068842, -5.558215102112974648 ) ) ;
#367 = CARTESIAN_POINT ( 'NONE',  ( -220.9628981692495699, 151.3494953986536018, 7.483278023344910324 ) ) ;
#368 = EDGE_LOOP ( 'NONE', ( #10873, #2288 ) ) ;
#369 = CARTESIAN_POINT ( 'NONE',  ( -219.7507648086670429, 149.4749995001899663, 9.873895959572530856 ) ) ;
#370 = ORIENTED_EDGE ( 'NONE', *, *, #1545, .F. ) ;
#371 = CARTESIAN_POINT ( 'NONE',  ( -168.7841562197520489, 125.8293614238909299, -3.029850393553606303 ) ) ;
#372 = FACE_OUTER_BOUND ( 'NONE', #12651, .T. ) ;
#373 = AXIS2_PLACEMENT_3D ( 'NONE', #13663, #6109, #10928 ) ;
#374 = EDGE_LOOP ( 'NONE', ( #1367, #9906 ) ) ;
#375 = CARTESIAN_POINT ( 'NONE',  ( 178.0000000000000853, -178.8058001507315566, 52.69066787724494816 ) ) ;
#376 = CARTESIAN_POINT ( 'NONE',  ( 19.11029453487719110, 40.04259805664093363, 7.600000000000002309 ) ) ;
#377 = VECTOR ( 'NONE', #4213, 1000.000000000000000 ) ;
#378 = CARTESIAN_POINT ( 'NONE',  ( 2.000000000000000000, -1.587713240271461546, 2.750000000000000000 ) ) ;
#379 = VERTEX_POINT ( 'NONE', #14473 ) ;
#380 = EDGE_CURVE ( 'NONE', #4418, #13651, #9757, .T. ) ;
#381 = PRODUCT_CONTEXT ( 'NONE', #8388, 'mechanical' ) ;
#382 = EDGE_LOOP ( 'NONE', ( #11195, #13930, #5127, #3542 ) ) ;
#383 = CARTESIAN_POINT ( 'NONE',  ( 177.5000000000000853, -178.8058001507315566, 52.19066787724494816 ) ) ;
#384 = DIRECTION ( 'NONE',  ( -0.000000000000000000, -0.000000000000000000, 1.000000000000000000 ) ) ;
#385 = EDGE_LOOP ( 'NONE', ( #10677, #7810, #419, #2894 ) ) ;
#386 = CARTESIAN_POINT ( 'NONE',  ( -217.3071532141029820, 141.4846410501804712, 2.431557144026069928 ) ) ;
#387 = AXIS2_PLACEMENT_3D ( 'NONE', #2185, #5898, #3681 ) ;
#388 = FACE_BOUND ( 'NONE', #1673, .T. ) ;
#389 = ORIENTED_EDGE ( 'NONE', *, *, #3413, .F. ) ;
#390 = ORIENTED_EDGE ( 'NONE', *, *, #8566, .T. ) ;
#391 = CARTESIAN_POINT ( 'NONE',  ( -85.99999999999994316, 62.13993994372673768, 13.30000000000175575 ) ) ;
#392 = EDGE_CURVE ( 'NONE', #873, #13090, #3748, .T. ) ;
#393 = CARTESIAN_POINT ( 'NONE',  ( 198.8872864542346974, 32.16591232847088122, -2.310211674251309688 ) ) ;
#394 = ORIENTED_EDGE ( 'NONE', *, *, #3261, .F. ) ;
#395 = CARTESIAN_POINT ( 'NONE',  ( -187.5347606140533969, 120.9941390333424636, 2.431555724346869063 ) ) ;
#396 = DIRECTION ( 'NONE',  ( 0.000000000000000000, 0.000000000000000000, -1.000000000000000000 ) ) ;
#397 = CARTESIAN_POINT ( 'NONE',  ( -156.1143961258770503, 109.3137364120441077, -4.543781140870884805 ) ) ;
#398 = DIRECTION ( 'NONE',  ( -1.000000000000000000, -0.000000000000000000, -0.000000000000000000 ) ) ;
#399 = CIRCLE ( 'NONE', #3701, 1.000000000000000888 ) ;
#400 = CARTESIAN_POINT ( 'NONE',  ( -76.50000000000004263, 16.03993994372673981, 24.94742576086838781 ) ) ;
#401 = EDGE_CURVE ( 'NONE', #462, #12631, #776, .T. ) ;
#402 = DIRECTION ( 'NONE',  ( -0.000000000000000000, 1.000000000000000000, -0.000000000000000000 ) ) ;
#403 = ORIENTED_EDGE ( 'NONE', *, *, #203, .F. ) ;
#404 = FACE_BOUND ( 'NONE', #3437, .T. ) ;
#405 = CARTESIAN_POINT ( 'NONE',  ( -217.9852252332578928, 152.6415593000486126, -3.308226381094188095 ) ) ;
#406 = CARTESIAN_POINT ( 'NONE',  ( -195.7742941377835280, 134.4381891934308442, -5.230826428279600648 ) ) ;
#407 = DIRECTION ( 'NONE',  ( -0.000000000000000000, -0.000000000000000000, 1.000000000000000000 ) ) ;
#408 = ORIENTED_EDGE ( 'NONE', *, *, #12361, .F. ) ;
#409 = CARTESIAN_POINT ( 'NONE',  ( -199.2256335332332640, 127.9713659812714042, 5.434137442415931218 ) ) ;
#410 = CARTESIAN_POINT ( 'NONE',  ( 194.8975446553719451, 47.93174114899129989, -1.867390259657528251 ) ) ;
#411 = VERTEX_POINT ( 'NONE', #1368 ) ;
#412 = DIRECTION ( 'NONE',  ( 1.000000000000000000, 0.000000000000000000, 0.000000000000000000 ) ) ;
#413 = CARTESIAN_POINT ( 'NONE',  ( -63.50000000000002842, 19.53993994372674337, 9.999999999999998224 ) ) ;
#414 = FACE_OUTER_BOUND ( 'NONE', #14323, .T. ) ;
#415 = ADVANCED_FACE ( 'NONE', ( #12037 ), #9890, .T. ) ;
#416 = DIRECTION ( 'NONE',  ( -0.000000000000000000, 1.000000000000000000, -0.000000000000000000 ) ) ;
#418 = ADVANCED_FACE ( 'NONE', ( #10869 ), #4776, .F. ) ;
#417 = ADVANCED_FACE ( 'NONE', ( #6046 ), #9121, .T. ) ;
#419 = ORIENTED_EDGE ( 'NONE', *, *, #12484, .T. ) ;
#420 = CYLINDRICAL_SURFACE ( 'NONE', #12715, 5.000000000000017764 ) ;
#421 = DIRECTION ( 'NONE',  ( 1.000000000000000000, 0.000000000000000000, -0.000000000000000000 ) ) ;
#422 = EDGE_CURVE ( 'NONE', #8299, #5528, #13370, .T. ) ;
#423 = CARTESIAN_POINT ( 'NONE',  ( 178.0000000000000853, 15.03993994372673804, 24.94742576086838781 ) ) ;
#424 = ORIENTED_EDGE ( 'NONE', *, *, #5483, .F. ) ;
#425 = FACE_OUTER_BOUND ( 'NONE', #2124, .T. ) ;
#426 = CIRCLE ( 'NONE', #15310, 0.5000000000000004441 ) ;
#427 = VERTEX_POINT ( 'NONE', #7398 ) ;
#428 = ORIENTED_EDGE ( 'NONE', *, *, #9080, .F. ) ;
#429 = CARTESIAN_POINT ( 'NONE',  ( -166.6414209516114795, 123.5128972754229011, 2.431557144026069928 ) ) ;
#430 = FACE_OUTER_BOUND ( 'NONE', #4920, .T. ) ;
#431 = AXIS2_PLACEMENT_3D ( 'NONE', #11990, #8295, #10275 ) ;
#432 = CARTESIAN_POINT ( 'NONE',  ( -70.00000000000000000, 17.53993994372673271, 45.99999999999998579 ) ) ;
#433 = CARTESIAN_POINT ( 'NONE',  ( -63.50000000000002842, -178.8753867012115961, -29.82329228561640022 ) ) ;
#434 = DIRECTION ( 'NONE',  ( 1.000000000000000000, 0.000000000000000000, 0.000000000000000000 ) ) ;
#435 = VERTEX_POINT ( 'NONE', #5016 ) ;
#436 = EDGE_CURVE ( 'NONE', #7205, #8201, #10784, .T. ) ;
#437 = CARTESIAN_POINT ( 'NONE',  ( -157.8787660911425803, 118.6941998492684149, 0.000000000000000000 ) ) ;
#438 = PRODUCT_DEFINITION_CONTEXT ( 'detailed design', #1607, 'design' ) ;
#439 = ADVANCED_FACE ( 'NONE', ( #5527 ), #13887, .F. ) ;
#440 = DIRECTION ( 'NONE',  ( 1.000000000000000000, 0.000000000000000000, 0.000000000000000000 ) ) ;
#441 = AXIS2_PLACEMENT_3D ( 'NONE', #3058, #8986, #15190 ) ;
#442 = CARTESIAN_POINT ( 'NONE',  ( 208.8124460758720033, 42.05191026284237665, -4.433604294307299298 ) ) ;
#443 = CARTESIAN_POINT ( 'NONE',  ( -224.5811800873043182, 144.8667753680073531, 1.831365460742872209 ) ) ;
#444 = ORIENTED_EDGE ( 'NONE', *, *, #9592, .F. ) ;
#445 = EDGE_CURVE ( 'NONE', #10124, #3324, #12383, .T. ) ;
#446 = CARTESIAN_POINT ( 'NONE',  ( -218.2326813014511799, 152.2161514369302324, 8.572300711411607210 ) ) ;
#447 = ORIENTED_EDGE ( 'NONE', *, *, #8449, .T. ) ;
#448 = CARTESIAN_POINT ( 'NONE',  ( -170.5205985377005220, 122.7182524358224640, -5.056862372992222632 ) ) ;
#449 = CARTESIAN_POINT ( 'NONE',  ( 184.0000000000000568, 19.53993994372674337, -10.99999999999999822 ) ) ;
#450 = ORIENTED_EDGE ( 'NONE', *, *, #1874, .F. ) ;
#451 = DIRECTION ( 'NONE',  ( 0.000000000000000000, 0.000000000000000000, -1.000000000000000000 ) ) ;
#452 = CARTESIAN_POINT ( 'NONE',  ( 122.5806775638430253, 45.00321902537314145, 7.600000000000002309 ) ) ;
#453 = AXIS2_PLACEMENT_3D ( 'NONE', #12309, #7594, #7753 ) ;
#454 = VECTOR ( 'NONE', #11405, 1000.000000000000114 ) ;
#455 = EDGE_CURVE ( 'NONE', #6271, #3832, #8131, .T. ) ;
#456 = DIRECTION ( 'NONE',  ( 0.000000000000000000, 0.000000000000000000, -1.000000000000000000 ) ) ;
#457 = VERTEX_POINT ( 'NONE', #4861 ) ;
#458 = APPLICATION_PROTOCOL_DEFINITION ( 'draft international standard', 'automotive_design', 1998, #15303 ) ;
#459 = ORIENTED_EDGE ( 'NONE', *, *, #5935, .T. ) ;
#460 = AXIS2_PLACEMENT_3D ( 'NONE', #7389, #8262, #9589 ) ;
#461 = DIRECTION ( 'NONE',  ( -1.000000000000000000, 0.000000000000000000, 0.000000000000000000 ) ) ;
#462 = VERTEX_POINT ( 'NONE', #13132 ) ;
#463 = CARTESIAN_POINT ( 'NONE',  ( 175.9483885134608272, -181.3058001507315566, 84.88378295107885663 ) ) ;
#464 = AXIS2_PLACEMENT_3D ( 'NONE', #11793, #3266, #8332 ) ;
#465 = CARTESIAN_POINT ( 'NONE',  ( 177.5000000000000853, 17.53993994372673626, 52.49999999999997868 ) ) ;
#466 = EDGE_LOOP ( 'NONE', ( #4763, #4256, #4464, #11811 ) ) ;
#467 = EDGE_LOOP ( 'NONE', ( #5925, #93, #1050, #7042 ) ) ;
#468 = LINE ( 'NONE', #553, #2479 ) ;
#469 = LINE ( 'NONE', #13437, #12129 ) ;
#470 = VERTEX_POINT ( 'NONE', #2334 ) ;
#471 = CARTESIAN_POINT ( 'NONE',  ( 198.8863654052626657, 49.55881746625484396, -3.681704842056328086 ) ) ;
#472 = CARTESIAN_POINT ( 'NONE',  ( -142.6037198098624685, 96.81775716765160666, 0.000000000000000000 ) ) ;
#473 = CIRCLE ( 'NONE', #10842, 3.525000000000000355 ) ;
#474 = VECTOR ( 'NONE', #4202, 1000.000000000000000 ) ;
#475 = DIRECTION ( 'NONE',  ( -1.000000000000000000, 0.000000000000000000, 0.000000000000000000 ) ) ;
#476 = FACE_OUTER_BOUND ( 'NONE', #10606, .T. ) ;
#477 = CARTESIAN_POINT ( 'NONE',  ( -76.00000000000004263, -178.6666270497714777, 53.18093594598651919 ) ) ;
#478 = VECTOR ( 'NONE', #15395, 1000.000000000000000 ) ;
#479 = DIRECTION ( 'NONE',  ( 1.000000000000000000, 0.000000000000000000, 0.000000000000000000 ) ) ;
#480 = VECTOR ( 'NONE', #1184, 1000.000000000000000 ) ;
#481 = ORIENTED_EDGE ( 'NONE', *, *, #8412, .F. ) ;
#482 = DIRECTION ( 'NONE',  ( -0.4873681696970814659, -0.8731965799097686221, 0.000000000000000000 ) ) ;
#483 = CARTESIAN_POINT ( 'NONE',  ( -221.4307639069678544, 146.2562371466928255, -4.592498632207916209 ) ) ;
#484 = AXIS2_PLACEMENT_3D ( 'NONE', #5944, #4676, #14380 ) ;
#485 = CARTESIAN_POINT ( 'NONE',  ( -176.9844935205031504, 127.5518652045528825, -4.662307221713766658 ) ) ;
#486 = DIRECTION ( 'NONE',  ( -1.000000000000000000, 0.000000000000000000, 0.000000000000000000 ) ) ;
#487 = ORIENTED_EDGE ( 'NONE', *, *, #5572, .T. ) ;
#488 = CARTESIAN_POINT ( 'NONE',  ( -173.0737465816261818, 117.4314230949052558, 7.694953281110847421 ) ) ;
#489 = CARTESIAN_POINT ( 'NONE',  ( 201.2644297667355886, 32.15691159195442594, -0.6119088838163699862 ) ) ;
#490 = ORIENTED_EDGE ( 'NONE', *, *, #10011, .F. ) ;
#491 = ADVANCED_FACE ( 'NONE', ( #11969 ), #1138, .F. ) ;
#492 = DIRECTION ( 'NONE',  ( 1.000000000000000000, 0.000000000000000000, 0.000000000000000000 ) ) ;
#493 = CARTESIAN_POINT ( 'NONE',  ( -33.09899788034579160, 48.72489408690345414, 7.600000000000002309 ) ) ;
#494 = DIRECTION ( 'NONE',  ( 0.000000000000000000, 0.9569673715906176215, 0.2901955370279575286 ) ) ;
#495 = AXIS2_PLACEMENT_3D ( 'NONE', #10525, #9661, #9579 ) ;
#496 = CIRCLE ( 'NONE', #12110, 0.5000000000000000000 ) ;
#497 = CARTESIAN_POINT ( 'NONE',  ( -35.99999999999995026, 59.53993994372674337, 13.30000000000139870 ) ) ;
#498 = ORIENTED_EDGE ( 'NONE', *, *, #7139, .T. ) ;
#499 = FACE_OUTER_BOUND ( 'NONE', #8321, .T. ) ;
#500 = CARTESIAN_POINT ( 'NONE',  ( -198.5721217036497990, 144.7598446228703324, 3.478855109513426580 ) ) ;
#501 = CARTESIAN_POINT ( 'NONE',  ( -76.00000000000001421, -179.8058001507315566, -17.50000000000002487 ) ) ;
#502 = CIRCLE ( 'NONE', #9361, 1.000000000000000888 ) ;
#503 = CARTESIAN_POINT ( 'NONE',  ( 0.000000000000000000, 0.000000000000000000, 0.000000000000000000 ) ) ;
#504 = ORIENTED_EDGE ( 'NONE', *, *, #12136, .F. ) ;
#505 = EDGE_CURVE ( 'NONE', #2386, #1610, #1044, .T. ) ;
#507 = LINE ( 'NONE', #14731, #10105 ) ;
#506 = VECTOR ( 'NONE', #7405, 1000.000000000000000 ) ;
#508 = ORIENTED_EDGE ( 'NONE', *, *, #8880, .F. ) ;
#509 = EDGE_LOOP ( 'NONE', ( #9428, #2544 ) ) ;
#510 = CARTESIAN_POINT ( 'NONE',  ( 190.0000000000000853, 15.03993994372673804, 38.07518420361041933 ) ) ;
#511 = CARTESIAN_POINT ( 'NONE',  ( 124.2806775638430281, 45.00321902537314145, 5.000000000000000000 ) ) ;
#512 = CARTESIAN_POINT ( 'NONE',  ( 194.0000000000000568, 64.53993994372673626, 10.00000000000000178 ) ) ;
#513 = ADVANCED_FACE ( 'NONE', ( #9255 ), #2959, .F. ) ;
#514 = PRESENTATION_STYLE_ASSIGNMENT (( #7896 ) ) ;
#515 = LINE ( 'NONE', #433, #1175 ) ;
#516 = PRODUCT_RELATED_PRODUCT_CATEGORY ( 'part', '', ( #690 ) ) ;
#517 = CARTESIAN_POINT ( 'NONE',  ( -219.4169908596040273, 154.1192310103966179, 2.706804888356528771 ) ) ;
#518 = EDGE_CURVE ( 'NONE', #13949, #12631, #4054, .T. ) ;
#519 = CARTESIAN_POINT ( 'NONE',  ( 21.71949999999999648, 0.000000000000000000, 1.500000000000000000 ) ) ;
#520 = ORIENTED_EDGE ( 'NONE', *, *, #10311, .F. ) ;
#521 = AXIS2_PLACEMENT_3D ( 'NONE', #14117, #9393, #14192 ) ;
#522 = CARTESIAN_POINT ( 'NONE',  ( 0.2456200930618607225, 1.587713240271468207, -2.750000000000000000 ) ) ;
#523 = AXIS2_PLACEMENT_3D ( 'NONE', #7628, #7709, #8968 ) ;
#524 = CARTESIAN_POINT ( 'NONE',  ( -61.94838851346079167, -179.3058001507315566, 84.88378295107887084 ) ) ;
#525 = CARTESIAN_POINT ( 'NONE',  ( 207.1194509196011495, 46.14302886020001182, -1.185720282267065828 ) ) ;
#526 = CARTESIAN_POINT ( 'NONE',  ( -64.00000000000002842, 15.10952649420676863, 9.557440204760682789 ) ) ;
#527 = ORIENTED_EDGE ( 'NONE', *, *, #1736, .T. ) ;
#528 = B_SPLINE_CURVE_WITH_KNOTS ( 'NONE', 3,
 ( #15104, #3195, #13773, #8026, #5416, #11414 ),
 .UNSPECIFIED., .F., .F.,
 ( 4, 2, 4 ),
 ( 0.002949915431443937870, 0.003753579573369721003, 0.004557243715295504136 ),
 .UNSPECIFIED. ) ;
#529 = CARTESIAN_POINT ( 'NONE',  ( -219.5915661803683463, 153.8064519195449407, 4.439938623566930254 ) ) ;
#530 = ORIENTED_EDGE ( 'NONE', *, *, #7219, .T. ) ;
#531 = CARTESIAN_POINT ( 'NONE',  ( -167.7969933075935387, 127.5980187394608549, 2.035704077629012954 ) ) ;
#532 = CARTESIAN_POINT ( 'NONE',  ( -76.50000000000004263, 16.03993994372673626, 38.07518420361041933 ) ) ;
#533 = TOROIDAL_SURFACE ( 'NONE', #1054, 1.000000000000000000, 0.5000000000000000000 ) ;
#534 = EDGE_CURVE ( 'NONE', #12538, #8345, #9996, .T. ) ;
#535 = ADVANCED_FACE ( 'NONE', ( #6521 ), #1971, .F. ) ;
#536 = ORIENTED_EDGE ( 'NONE', *, *, #7965, .T. ) ;
#537 = EDGE_CURVE ( 'NONE', #9039, #10463, #3828, .T. ) ;
#538 = CARTESIAN_POINT ( 'NONE',  ( 70.26535645333922275, 38.79159067395544014, 10.00000000000000178 ) ) ;
#539 = DIRECTION ( 'NONE',  ( 0.000000000000000000, 0.000000000000000000, 1.000000000000000000 ) ) ;
#540 = FACE_OUTER_BOUND ( 'NONE', #6429, .T. ) ;
#541 = ORIENTED_EDGE ( 'NONE', *, *, #1567, .F. ) ;
#542 = CONTEXT_DEPENDENT_SHAPE_REPRESENTATION ( #7274, #13052 ) ;
#543 = MECHANICAL_DESIGN_GEOMETRIC_PRESENTATION_REPRESENTATION (  '', ( #10911 ), #10658 ) ;
#544 = ORIENTED_EDGE ( 'NONE', *, *, #8820, .T. ) ;
#545 = CARTESIAN_POINT ( 'NONE',  ( -83.77455057502459113, 65.19100426474074084, 0.000000000000000000 ) ) ;
#546 = ORIENTED_EDGE ( 'NONE', *, *, #11091, .T. ) ;
#547 = CLOSED_SHELL ( 'NONE', ( #13923, #14725, #1343, #11232, #3493, #10653, #12710, #1912, #4244, #2083, #9242, #12419, #15408, #10431, #12199, #12057, #3318, #15550, #7489, #14627 ) ) ;
#548 = DIRECTION ( 'NONE',  ( -1.000000000000000000, 0.000000000000000000, 0.000000000000000000 ) ) ;
#549 = EDGE_CURVE ( 'NONE', #10298, #12812, #1611, .T. ) ;
#550 = CARTESIAN_POINT ( 'NONE',  ( -1.048203272227196275E-15, -2.516314840832718502, -1.141614847838140490 ) ) ;
#551 = ORIENTED_EDGE ( 'NONE', *, *, #13799, .F. ) ;
#552 = VERTEX_POINT ( 'NONE', #6443 ) ;
#553 = CARTESIAN_POINT ( 'NONE',  ( -64.00000000000002842, 15.53993994372674159, -17.50000000000002487 ) ) ;
#554 = CARTESIAN_POINT ( 'NONE',  ( 114.0000000000000426, 15.03993994372673804, 38.07518420361041933 ) ) ;
#555 = VERTEX_POINT ( 'NONE', #2885 ) ;
#556 = SHAPE_REPRESENTATION ( 'Upper Moving Shear Blade Bar', ( #12337 ), #11555 ) ;
#557 = CARTESIAN_POINT ( 'NONE',  ( 205.4319281802536068, 33.87189768065903905, -1.932853472788024440 ) ) ;
#558 = DIRECTION ( 'NONE',  ( 0.000000000000000000, 1.000000000000000000, 6.938893903907227145E-17 ) ) ;
#559 = DIRECTION ( 'NONE',  ( -5.518327896226364679E-17, 0.9902680687415713612, -0.1391731009600582492 ) ) ;
#560 = DIRECTION ( 'NONE',  ( -0.000000000000000000, 1.000000000000000000, -0.000000000000000000 ) ) ;
#561 = AXIS2_PLACEMENT_3D ( 'NONE', #1268, #5934, #15618 ) ;
#562 = LINE ( 'NONE', #5161, #14608 ) ;
#563 = MANIFOLD_SOLID_BREP ( 'Boss-Extrude1', #14676 ) ;
#564 = PRODUCT_DEFINITION_SHAPE ( 'NONE', 'NONE',  #12586 ) ;
#565 = VECTOR ( 'NONE', #10580, 1000.000000000000000 ) ;
#566 = CARTESIAN_POINT ( 'NONE',  ( 202.1731860119849102, 31.08132011834958419, -8.150590381057213563 ) ) ;
#567 = EDGE_CURVE ( 'NONE', #8004, #6496, #10133, .T. ) ;
#568 = EDGE_LOOP ( 'NONE', ( #1581, #6786, #11329, #3119, #5472 ) ) ;
#569 = DIRECTION ( 'NONE',  ( 1.000000000000000000, 0.000000000000000000, 0.000000000000000000 ) ) ;
#570 = CARTESIAN_POINT ( 'NONE',  ( -202.8891874331996519, 144.7632710727894505, -2.963320117457099112 ) ) ;
#571 = DIRECTION ( 'NONE',  ( -1.000000000000000000, -2.751328491981765035E-32, 3.965082230804130220E-16 ) ) ;
#572 = ORIENTED_EDGE ( 'NONE', *, *, #10492, .T. ) ;
#573 = CARTESIAN_POINT ( 'NONE',  ( -186.4931015233695462, 122.8215886266871593, 7.918248976830652097 ) ) ;
#574 = UNCERTAINTY_MEASURE_WITH_UNIT (LENGTH_MEASURE( 1.000000000000000082E-05 ), #14890, 'distance_accuracy_value', 'NONE');
#575 = CARTESIAN_POINT ( 'NONE',  ( 207.3546231538492179, 50.29643094772573164, -2.498001438440778710 ) ) ;
#576 = VECTOR ( 'NONE', #13961, 1000.000000000000000 ) ;
#577 = EDGE_LOOP ( 'NONE', ( #6152, #5245, #8146, #7504 ) ) ;
#578 = AXIS2_PLACEMENT_3D ( 'NONE', #12146, #8381, #196 ) ;
#579 = CARTESIAN_POINT ( 'NONE',  ( 2.000000000000000000, -3.175426480542940411, 0.000000000000000000 ) ) ;
#580 = LINE ( 'NONE', #12899, #7977 ) ;
#581 = LINE ( 'NONE', #14871, #3041 ) ;
#582 = CARTESIAN_POINT ( 'NONE',  ( -64.00000000000002842, 16.03993994372673626, 52.49999999999997868 ) ) ;
#583 = ORIENTED_EDGE ( 'NONE', *, *, #567, .T. ) ;
#584 = DIRECTION ( 'NONE',  ( 1.000000000000000000, 2.751328491981765035E-32, -3.965082230804130220E-16 ) ) ;
#585 = CIRCLE ( 'NONE', #7676, 0.4999999999999996114 ) ;
#586 = CARTESIAN_POINT ( 'NONE',  ( -182.6699909761611877, 123.4132960977408970, 9.577123744044220288 ) ) ;
#587 = DIRECTION ( 'NONE',  ( 3.965082230804130220E-16, 0.000000000000000000, -1.000000000000000000 ) ) ;
#588 = CARTESIAN_POINT ( 'NONE',  ( -156.1569890673251280, 111.0783851182460893, -4.963902819945231748 ) ) ;
#589 = ORIENTED_EDGE ( 'NONE', *, *, #6377, .F. ) ;
#590 = LINE ( 'NONE', #14959, #5579 ) ;
#591 = VERTEX_POINT ( 'NONE', #3904 ) ;
#592 = VERTEX_POINT ( 'NONE', #2722 ) ;
#593 = B_SPLINE_CURVE_WITH_KNOTS ( 'NONE', 3,
 ( #14279, #11773, #13093, #6006, #2212, #5766 ),
 .UNSPECIFIED., .F., .F.,
 ( 4, 2, 4 ),
 ( 0.008690415895085797093, 0.01102883710845593487, 0.01336725832182607265 ),
 .UNSPECIFIED. ) ;
#594 = CARTESIAN_POINT ( 'NONE',  ( -150.6118892440573802, 107.8916133795084846, 9.813105602333695998 ) ) ;
#595 = CARTESIAN_POINT ( 'NONE',  ( -164.5262273476079713, 106.7842295329138835, 5.000000000000000000 ) ) ;
#596 = ADVANCED_FACE ( 'NONE', ( #3241, #7547, #404, #10066, #5321, #12343, #1529 ), #6365, .T. ) ;
#597 = VECTOR ( 'NONE', #13500, 1000.000000000000000 ) ;
#598 = CARTESIAN_POINT ( 'NONE',  ( 14.00000000000004086, 64.51493994372674479, 11.50000000000105160 ) ) ;
#599 = CARTESIAN_POINT ( 'NONE',  ( -169.3917585582371714, 124.7407464570165700, 8.854531459401838944 ) ) ;
#600 = CARTESIAN_POINT ( 'NONE',  ( -219.0516113763855799, 154.7738657095153769, -1.749095451262919765 ) ) ;
#601 = CIRCLE ( 'NONE', #13716, 3.500000000000003109 ) ;
#602 = CARTESIAN_POINT ( 'NONE',  ( -70.00000000000000000, -179.3058001507315566, 77.95141194869098911 ) ) ;
#603 = DIRECTION ( 'NONE',  ( 1.000000000000000000, 0.000000000000000000, 0.000000000000000000 ) ) ;
#604 = PRODUCT_DEFINITION_CONTEXT ( 'detailed design', #12686, 'design' ) ;
#605 = FACE_OUTER_BOUND ( 'NONE', #8179, .T. ) ;
#606 = AXIS2_PLACEMENT_3D ( 'NONE', #2740, #184, #1548 ) ;
#607 = ADVANCED_FACE ( 'NONE', ( #2807 ), #5240, .T. ) ;
#608 = CARTESIAN_POINT ( 'NONE',  ( 200.1062858801516597, 40.86394065090267702, 12.00000000000001066 ) ) ;
#609 = CARTESIAN_POINT ( 'NONE',  ( 190.0000000000000568, 16.03993994372673981, -17.50000000000002487 ) ) ;
#610 = EDGE_LOOP ( 'NONE', ( #2494, #13099, #11658, #12141 ) ) ;
#611 = CARTESIAN_POINT ( 'NONE',  ( -220.4620190166787950, 152.2468990252863819, 9.155722436418765042 ) ) ;
#612 = ORIENTED_EDGE ( 'NONE', *, *, #2131, .T. ) ;
#613 = CARTESIAN_POINT ( 'NONE',  ( 114.0000000000000568, 59.53993994372674337, 15.00000000000035172 ) ) ;
#614 = CARTESIAN_POINT ( 'NONE',  ( 185.1062858801516882, 55.86394065090267702, 18.00000000000000355 ) ) ;
#615 = ORIENTED_EDGE ( 'NONE', *, *, #12398, .F. ) ;
#616 = DIRECTION ( 'NONE',  ( 0.000000000000000000, 0.000000000000000000, 1.000000000000000000 ) ) ;
#617 = LINE ( 'NONE', #4250, #8359 ) ;
#618 = VECTOR ( 'NONE', #13285, 1000.000000000000114 ) ;
#619 = DIRECTION ( 'NONE',  ( 1.000000000000000000, 0.000000000000000000, 0.000000000000000000 ) ) ;
#620 = VERTEX_POINT ( 'NONE', #1173 ) ;
#621 = ORIENTED_EDGE ( 'NONE', *, *, #1015, .F. ) ;
#622 = EDGE_CURVE ( 'NONE', #2293, #7132, #13393, .T. ) ;
#623 = CARTESIAN_POINT ( 'NONE',  ( 203.1375244286944906, 48.81137831324044640, 0.6531691591918254991 ) ) ;
#625 = EDGE_CURVE ( 'NONE', #15030, #13622, #4821, .T. ) ;
#624 = EDGE_CURVE ( 'NONE', #8392, #8751, #593, .T. ) ;
#626 = FACE_OUTER_BOUND ( 'NONE', #9253, .T. ) ;
#627 = VERTEX_POINT ( 'NONE', #2292 ) ;
#628 = CARTESIAN_POINT ( 'NONE',  ( -76.50000000000001421, -179.8058001507315566, -30.31842631998718574 ) ) ;
#629 = VECTOR ( 'NONE', #6503, 1000.000000000000114 ) ;
#630 = CARTESIAN_POINT ( 'NONE',  ( 0.02351960456806068828, -2.650883748492876446, -0.9085346626517005753 ) ) ;
#631 = ORIENTED_EDGE ( 'NONE', *, *, #14587, .T. ) ;
#632 = ORIENTED_EDGE ( 'NONE', *, *, #3155, .T. ) ;
#633 = CARTESIAN_POINT ( 'NONE',  ( -31.27399788034579586, 48.72489408690345414, 10.00000000000000178 ) ) ;
#634 = VECTOR ( 'NONE', #8882, 1000.000000000000000 ) ;
#635 = CARTESIAN_POINT ( 'NONE',  ( 190.0000000000000853, -178.9449732516916072, 64.32815825124538378 ) ) ;
#636 = ORIENTED_EDGE ( 'NONE', *, *, #225, .T. ) ;
#637 = CARTESIAN_POINT ( 'NONE',  ( 0.7145311798163155315, -4.618802153516981868, 8.000000000000007105 ) ) ;
#638 = DIRECTION ( 'NONE',  ( 0.000000000000000000, -0.000000000000000000, -1.000000000000000000 ) ) ;
#639 = DIRECTION ( 'NONE',  ( 0.000000000000000000, 0.000000000000000000, -1.000000000000000000 ) ) ;
#640 = CARTESIAN_POINT ( 'NONE',  ( -76.00000000000001421, -178.7362136002515172, -17.68580191161595394 ) ) ;
#641 = DIRECTION ( 'NONE',  ( 0.000000000000000000, 0.000000000000000000, 1.000000000000000000 ) ) ;
#642 = MANIFOLD_SOLID_BREP ( 'Sweep1', #13662 ) ;
#643 = CIRCLE ( 'NONE', #1402, 5.400000000000019007 ) ;
#644 = DIRECTION ( 'NONE',  ( 0.000000000000000000, -1.000000000000000000, 0.000000000000000000 ) ) ;
#645 = VERTEX_POINT ( 'NONE', #14203 ) ;
#646 = CARTESIAN_POINT ( 'NONE',  ( 114.0000000000000568, 59.53993994372674337, 13.30000000000035776 ) ) ;
#647 = CARTESIAN_POINT ( 'NONE',  ( -187.0868153883506011, 133.8486679469899343, -4.640918829492425957 ) ) ;
#648 = DIRECTION ( 'NONE',  ( 0.000000000000000000, 0.000000000000000000, -1.000000000000000000 ) ) ;
#649 = VERTEX_POINT ( 'NONE', #14359 ) ;
#650 = CARTESIAN_POINT ( 'NONE',  ( -214.6174474432871762, 135.6318802667844921, 5.434137442415934771 ) ) ;
#651 = CARTESIAN_POINT ( 'NONE',  ( 211.8663679066739007, 39.14335912920272875, 0.001962313962203070510 ) ) ;
#652 = VERTEX_POINT ( 'NONE', #11928 ) ;
#653 = AXIS2_PLACEMENT_3D ( 'NONE', #7411, #179, #5028 ) ;
#654 = CARTESIAN_POINT ( 'NONE',  ( 166.7445055987502656, 66.43865443379107205, -0.9107274384406879308 ) ) ;
#655 = CARTESIAN_POINT ( 'NONE',  ( 21.99999999999999289, 0.000000000000000000, 0.000000000000000000 ) ) ;
#656 = CARTESIAN_POINT ( 'NONE',  ( -33.09899788034579871, 48.72489408690345414, 10.00000000000000178 ) ) ;
#657 = EDGE_CURVE ( 'NONE', #11157, #14585, #9638, .T. ) ;
#658 = CARTESIAN_POINT ( 'NONE',  ( 190.5000000000000568, -179.2362136002515172, -18.26098611522645498 ) ) ;
#659 = EDGE_LOOP ( 'NONE', ( #14595, #131 ) ) ;
#660 = CARTESIAN_POINT ( 'NONE',  ( 184.0000000000000568, -201.3058001507315566, 76.45141194869098911 ) ) ;
#661 = CARTESIAN_POINT ( 'NONE',  ( -191.1905365997726562, 133.0085349363843363, 10.16010209732750624 ) ) ;
#662 = FACE_OUTER_BOUND ( 'NONE', #4108, .T. ) ;
#663 = CARTESIAN_POINT ( 'NONE',  ( -155.8520457446764453, 110.8171731141052163, -4.950117075408069667 ) ) ;
#664 = ORIENTED_EDGE ( 'NONE', *, *, #6908, .T. ) ;
#665 = DIRECTION ( 'NONE',  ( 0.000000000000000000, 0.000000000000000000, 1.000000000000000000 ) ) ;
#666 = ORIENTED_EDGE ( 'NONE', *, *, #11149, .F. ) ;
#667 = ORIENTED_EDGE ( 'NONE', *, *, #9159, .T. ) ;
#668 = DIRECTION ( 'NONE',  ( 0.000000000000000000, 0.000000000000000000, -1.000000000000000000 ) ) ;
#669 = DIRECTION ( 'NONE',  ( -0.000000000000000000, 1.000000000000000000, -0.000000000000000000 ) ) ;
#670 = CARTESIAN_POINT ( 'NONE',  ( 164.0000000000000568, 62.13993994372673768, 15.00000000000000355 ) ) ;
#671 = CARTESIAN_POINT ( 'NONE',  ( -169.9972604110092789, 123.6558948400181634, 9.476346162107795124 ) ) ;
#672 = CARTESIAN_POINT ( 'NONE',  ( -218.9426345149119300, 150.9185095621452035, -4.524781484457172986 ) ) ;
#673 = CARTESIAN_POINT ( 'NONE',  ( -130.9946291778373961, 96.97121815129470690, 5.000000000000000000 ) ) ;
#674 = DIRECTION ( 'NONE',  ( 3.965082230804130220E-16, 0.000000000000000000, -1.000000000000000000 ) ) ;
#675 = DIRECTION ( 'NONE',  ( -0.000000000000000000, -0.000000000000000000, 1.000000000000000000 ) ) ;
#676 = ADVANCED_FACE ( 'NONE', ( #7123 ), #8237, .T. ) ;
#677 = FACE_OUTER_BOUND ( 'NONE', #3082, .T. ) ;
#678 = AXIS2_PLACEMENT_3D ( 'NONE', #4721, #11915, #10972 ) ;
#679 = FACE_BOUND ( 'NONE', #3096, .T. ) ;
#680 = DIRECTION ( 'NONE',  ( 1.000000000000000000, 0.000000000000000000, 0.000000000000000000 ) ) ;
#681 = EDGE_CURVE ( 'NONE', #5691, #12864, #13249, .T. ) ;
#682 = ORIENTED_EDGE ( 'NONE', *, *, #14233, .T. ) ;
#683 = AXIS2_PLACEMENT_3D ( 'NONE', #8224, #1001, #14265 ) ;
#684 = ORIENTED_EDGE ( 'NONE', *, *, #4682, .F. ) ;
#685 = CARTESIAN_POINT ( 'NONE',  ( -173.9738588760758944, 116.5311944691898560, -0.9961046041182962663 ) ) ;
#686 = FACE_OUTER_BOUND ( 'NONE', #769, .T. ) ;
#687 = FACE_OUTER_BOUND ( 'NONE', #13168, .T. ) ;
#688 = DIRECTION ( 'NONE',  ( 0.6130913241491352528, 0.7900120431063440973, -6.390853288732736916E-17 ) ) ;
#689 = DIRECTION ( 'NONE',  ( 1.000000000000000000, 0.000000000000000000, 0.000000000000000000 ) ) ;
#690 = PRODUCT ( 'Recoil spring', 'Recoil spring', '', ( #15067 ) ) ;
#691 = ADVANCED_FACE ( 'NONE', ( #3556 ), #4497, .F. ) ;
#692 = VECTOR ( 'NONE', #1638, 1000.000000000000000 ) ;
#693 = FACE_OUTER_BOUND ( 'NONE', #15416, .T. ) ;
#694 = ORIENTED_EDGE ( 'NONE', *, *, #8736, .F. ) ;
#695 = AXIS2_PLACEMENT_3D ( 'NONE', #4147, #10396, #5501 ) ;
#696 = APPLICATION_PROTOCOL_DEFINITION ( 'draft international standard', 'automotive_design', 1998, #12900 ) ;
#697 = ORIENTED_EDGE ( 'NONE', *, *, #1397, .T. ) ;
#698 = ORIENTED_EDGE ( 'NONE', *, *, #5084, .T. ) ;
#699 = FACE_BOUND ( 'NONE', #1042, .T. ) ;
#700 = CARTESIAN_POINT ( 'NONE',  ( -225.6985468192879409, 142.8648374703979016, 2.076118051499458161 ) ) ;
#701 = VERTEX_POINT ( 'NONE', #11853 ) ;
#702 = ORIENTED_EDGE ( 'NONE', *, *, #1006, .F. ) ;
#703 = CARTESIAN_POINT ( 'NONE',  ( 190.5000000000000568, -179.8058001507315566, -17.19066787724516843 ) ) ;
#704 = PRODUCT_DEFINITION_FORMATION_WITH_SPECIFIED_SOURCE ( 'ANY', '', #10548, .NOT_KNOWN. ) ;
#705 = EDGE_CURVE ( 'NONE', #14207, #5229, #14437, .T. ) ;
#706 = DIRECTION ( 'NONE',  ( -1.000000000000000000, 0.000000000000000000, 0.000000000000000000 ) ) ;
#707 = VECTOR ( 'NONE', #4697, 1000.000000000000000 ) ;
#708 = EDGE_LOOP ( 'NONE', ( #6506, #5405, #10280, #13729 ) ) ;
#709 = CARTESIAN_POINT ( 'NONE',  ( 205.5168546899054434, 47.82311440310952833, -1.064259200291542529 ) ) ;
#710 = DIRECTION ( 'NONE',  ( 1.000000000000000000, -2.751328491981765035E-32, 3.965082230804130220E-16 ) ) ;
#711 = DIRECTION ( 'NONE',  ( 1.000000000000000000, 0.000000000000000000, 0.000000000000000000 ) ) ;
#712 = DIRECTION ( 'NONE',  ( 1.000000000000000000, 0.000000000000000000, -0.000000000000000000 ) ) ;
#713 = APPLICATION_CONTEXT ( 'automotive_design' ) ;
#714 = EDGE_CURVE ( 'NONE', #5220, #7650, #15299, .T. ) ;
#715 = EDGE_CURVE ( 'NONE', #10772, #8234, #3323, .T. ) ;
#716 = CARTESIAN_POINT ( 'NONE',  ( -70.00000000000000000, 17.53993994372673271, 47.49999999999997868 ) ) ;
#717 = ADVANCED_FACE ( 'NONE', ( #1332, #7434 ), #1486, .F. ) ;
#718 = AXIS2_PLACEMENT_3D ( 'NONE', #1049, #5716, #8108 ) ;
#719 = LINE ( 'NONE', #10143, #474 ) ;
#720 = VERTEX_POINT ( 'NONE', #9959 ) ;
#721 = CARTESIAN_POINT ( 'NONE',  ( -155.6477983077465410, 110.1970436846185066, 84.88378295107887084 ) ) ;
#722 = CARTESIAN_POINT ( 'NONE',  ( -169.4320859569187405, 123.9702250307836238, -4.722862203412457660 ) ) ;
#723 = FACE_OUTER_BOUND ( 'NONE', #9664, .T. ) ;
#724 = EDGE_LOOP ( 'NONE', ( #6088, #7663, #14419, #15071, #11022 ) ) ;
#725 = CARTESIAN_POINT ( 'NONE',  ( -195.7742941377835280, 134.4381891934308442, -5.230826428279600648 ) ) ;
#726 = UNCERTAINTY_MEASURE_WITH_UNIT (LENGTH_MEASURE( 1.000000000000000082E-05 ), #3698, 'distance_accuracy_value', 'NONE');
#727 = CARTESIAN_POINT ( 'NONE',  ( 201.6516474359912934, 52.64960446646696113, -8.385050746608255778 ) ) ;
#728 = AXIS2_PLACEMENT_3D ( 'NONE', #4128, #8966, #3036 ) ;
#729 = EDGE_LOOP ( 'NONE', ( #13768, #13485, #6754, #10532 ) ) ;
#730 = AXIS2_PLACEMENT_3D ( 'NONE', #1202, #9673, #13125 ) ;
#731 = EDGE_CURVE ( 'NONE', #11157, #8697, #65, .T. ) ;
#732 = CARTESIAN_POINT ( 'NONE',  ( 0.2456200930618629430, 3.175426480542944407, 1.454290997841272695E-16 ) ) ;
#733 = DIRECTION ( 'NONE',  ( 0.000000000000000000, 0.000000000000000000, 1.000000000000000000 ) ) ;
#734 = EDGE_CURVE ( 'NONE', #12823, #5329, #1812, .T. ) ;
#735 = CARTESIAN_POINT ( 'NONE',  ( -152.4086188282879277, 107.2728346664360402, -4.548387523817075895 ) ) ;
#736 = VECTOR ( 'NONE', #8355, 999.9999999999998863 ) ;
#737 = AXIS2_PLACEMENT_3D ( 'NONE', #10217, #240, #15526 ) ;
#738 = CARTESIAN_POINT ( 'NONE',  ( -105.7032403413611661, 68.63699971342407480, 10.00000000000000178 ) ) ;
#739 = ORIENTED_EDGE ( 'NONE', *, *, #8236, .F. ) ;
#740 = AXIS2_PLACEMENT_3D ( 'NONE', #3109, #8013, #15241 ) ;
#741 = CYLINDRICAL_SURFACE ( 'NONE', #7444, 3.500000000000001332 ) ;
#742 = CARTESIAN_POINT ( 'NONE',  ( -174.5069932933876942, 126.2863744793834826, 9.536681319450917016 ) ) ;
#743 = DIRECTION ( 'NONE',  ( -1.000000000000000000, 0.000000000000000000, 0.000000000000000000 ) ) ;
#744 = CARTESIAN_POINT ( 'NONE',  ( -157.1749258454821927, 111.0568882623570062, -4.859112388478813216 ) ) ;
#745 = ORIENTED_EDGE ( 'NONE', *, *, #9421, .T. ) ;
#746 = LINE ( 'NONE', #15426, #3814 ) ;
#747 = EDGE_CURVE ( 'NONE', #6193, #15197, #6107, .T. ) ;
#748 = EDGE_LOOP ( 'NONE', ( #9743, #1718 ) ) ;
#749 = ORIENTED_EDGE ( 'NONE', *, *, #705, .F. ) ;
#750 = AXIS2_PLACEMENT_3D ( 'NONE', #11545, #7934, #3105 ) ;
#751 = CARTESIAN_POINT ( 'NONE',  ( 122.5806775638430253, 45.00321902537314145, 10.00000000000000178 ) ) ;
#752 = LINE ( 'NONE', #5511, #3482 ) ;
#753 = CIRCLE ( 'NONE', #1005, 3.525000000000000355 ) ;
#754 = AXIS2_PLACEMENT_3D ( 'NONE', #3682, #1381, #6219 ) ;
#755 = CARTESIAN_POINT ( 'NONE',  ( 64.00000000000005684, 64.53993994372673626, 15.00000000000070166 ) ) ;
#756 = CARTESIAN_POINT ( 'NONE',  ( -173.9115424460105430, 116.6428441356814432, 5.774694861875956597 ) ) ;
#757 = CARTESIAN_POINT ( 'NONE',  ( -222.4281468042453298, 148.7242724638446703, -5.036090039102246507 ) ) ;
#758 = CARTESIAN_POINT ( 'NONE',  ( -64.00000000000002842, -178.8058001507315566, -17.19066787724516843 ) ) ;
#759 = CARTESIAN_POINT ( 'NONE',  ( 184.0000000000000568, 17.53993994372673271, 47.49999999999997868 ) ) ;
#760 = CIRCLE ( 'NONE', #10878, 17.06579782980005433 ) ;
#761 = DIRECTION ( 'NONE',  ( 0.000000000000000000, -6.938893903907222067E-15, 1.000000000000000000 ) ) ;
#762 = AXIS2_PLACEMENT_3D ( 'NONE', #942, #1027, #8085 ) ;
#763 = DIRECTION ( 'NONE',  ( -1.000000000000000000, -0.000000000000000000, -0.000000000000000000 ) ) ;
#764 = DIRECTION ( 'NONE',  ( 0.000000000000000000, 0.000000000000000000, -1.000000000000000000 ) ) ;
#765 = EDGE_CURVE ( 'NONE', #9030, #14554, #2287, .T. ) ;
#766 = CARTESIAN_POINT ( 'NONE',  ( -219.7707515679132655, 153.4854131703968392, -0.3598758019112536233 ) ) ;
#767 = ORIENTED_EDGE ( 'NONE', *, *, #14509, .T. ) ;
#768 = CYLINDRICAL_SURFACE ( 'NONE', #9832, 1.699999999999993072 ) ;
#769 = EDGE_LOOP ( 'NONE', ( #6172, #937, #13033, #15405 ) ) ;
#770 = CARTESIAN_POINT ( 'NONE',  ( 0.08224679563972137064, -7.710515798486379246, -2.644994884459106466 ) ) ;
#771 = CARTESIAN_POINT ( 'NONE',  ( -85.27455057502459113, 65.19100426474074084, 10.00000000000000178 ) ) ;
#772 = ORIENTED_EDGE ( 'NONE', *, *, #9707, .F. ) ;
#773 = CARTESIAN_POINT ( 'NONE',  ( -170.1275826011421941, 128.8939672761866859, 2.500000000760459695 ) ) ;
#774 = CARTESIAN_POINT ( 'NONE',  ( 64.00000000000005684, 64.53993994372673626, 11.47500000000070131 ) ) ;
#775 = CIRCLE ( 'NONE', #5318, 8.000000000000028422 ) ;
#776 = CIRCLE ( 'NONE', #15400, 5.000000000000004441 ) ;
#777 = CARTESIAN_POINT ( 'NONE',  ( 178.0000000000000853, -178.7362136002515172, 52.68580191161573367 ) ) ;
#778 = ORIENTED_EDGE ( 'NONE', *, *, #7223, .T. ) ;
#779 = ORIENTED_EDGE ( 'NONE', *, *, #13958, .F. ) ;
#780 = CARTESIAN_POINT ( 'NONE',  ( 207.3736904795575811, 50.31851200600168994, -2.642755332960478043 ) ) ;
#781 = CARTESIAN_POINT ( 'NONE',  ( -64.00000000000002842, -178.8058001507315566, 52.19066787724494816 ) ) ;
#782 = ORIENTED_EDGE ( 'NONE', *, *, #1484, .F. ) ;
#783 = CARTESIAN_POINT ( 'NONE',  ( 178.0000000000000853, -178.7362136002515172, -17.68580191161595394 ) ) ;
#784 = CIRCLE ( 'NONE', #4837, 8.000000000000028422 ) ;
#785 = APPLICATION_CONTEXT ( 'automotive_design' ) ;
#786 = DIRECTION ( 'NONE',  ( 0.000000000000000000, 0.000000000000000000, 1.000000000000000000 ) ) ;
#787 = EDGE_LOOP ( 'NONE', ( #6983, #4310, #14077, #11881 ) ) ;
#788 = EDGE_LOOP ( 'NONE', ( #3520, #15305, #7596, #11160 ) ) ;
#789 = AXIS2_PLACEMENT_3D ( 'NONE', #609, #10339, #13796 ) ;
#790 = DIRECTION ( 'NONE',  ( -1.000000000000000000, 0.000000000000000000, 0.000000000000000000 ) ) ;
#791 = EDGE_CURVE ( 'NONE', #2861, #14616, #12302, .T. ) ;
#792 = DIRECTION ( 'NONE',  ( 0.000000000000000000, -1.486905836551548832E-16, 1.000000000000000000 ) ) ;
#793 = ORIENTED_EDGE ( 'NONE', *, *, #9332, .T. ) ;
#794 = CARTESIAN_POINT ( 'NONE',  ( 14.00000000000004086, 59.53993994372674337, 15.00000000000104983 ) ) ;
#795 = LINE ( 'NONE', #4513, #5561 ) ;
#796 = DIRECTION ( 'NONE',  ( 0.000000000000000000, -1.000000000000000000, 0.000000000000000000 ) ) ;
#797 = CARTESIAN_POINT ( 'NONE',  ( 184.0000000000000568, 15.53993994372673981, -13.99999999999999112 ) ) ;
#798 = CARTESIAN_POINT ( 'NONE',  ( -64.00000000000002842, -178.8058001507315566, -17.19066787724516843 ) ) ;
#799 = COLOUR_RGB ( '', 0.66274510, 0.83137255, 0.94901961) ;
#800 = AXIS2_PLACEMENT_3D ( 'NONE', #12219, #14347, #9547 ) ;
#801 = DIRECTION ( 'NONE',  ( 0.000000000000000000, -1.000000000000000000, -4.956352788505160310E-17 ) ) ;
#802 = ORIENTED_EDGE ( 'NONE', *, *, #15381, .T. ) ;
#803 = DIRECTION ( 'NONE',  ( -0.000000000000000000, -0.000000000000000000, 1.000000000000000000 ) ) ;
#804 = EDGE_CURVE ( 'NONE', #3126, #11344, #6868, .T. ) ;
#805 = CARTESIAN_POINT ( 'NONE',  ( -170.8299300849453459, 127.1729693371208043, -2.992655347556774981 ) ) ;
#806 = DIRECTION ( 'NONE',  ( -0.000000000000000000, -0.9902680687415713612, 0.1391731009600582492 ) ) ;
#807 = ORIENTED_EDGE ( 'NONE', *, *, #7985, .T. ) ;
#808 = CARTESIAN_POINT ( 'NONE',  ( -219.6417540138374704, 145.3326194796887023, -4.642206099735023628 ) ) ;
#809 = CARTESIAN_POINT ( 'NONE',  ( 188.2965488188713721, 39.35787245461563089, -4.374714073396582137 ) ) ;
#810 = VERTEX_POINT ( 'NONE', #13328 ) ;
#811 = AXIS2_PLACEMENT_3D ( 'NONE', #8478, #2543, #7216 ) ;
#812 = DIRECTION ( 'NONE',  ( -1.000000000000000000, -1.669238443041287429E-16, 0.000000000000000000 ) ) ;
#813 = CARTESIAN_POINT ( 'NONE',  ( 0.000000000000000000, -7.511572993685817836E-16, 2.749999999999999112 ) ) ;
#814 = LINE ( 'NONE', #11569, #14126 ) ;
#815 = VERTEX_POINT ( 'NONE', #2530 ) ;
#816 = DIRECTION ( 'NONE',  ( 0.000000000000000000, 0.000000000000000000, -1.000000000000000000 ) ) ;
#817 = AXIS2_PLACEMENT_3D ( 'NONE', #1888, #15144, #9176 ) ;
#818 = ORIENTED_EDGE ( 'NONE', *, *, #8671, .T. ) ;
#819 = CARTESIAN_POINT ( 'NONE',  ( 200.1062858801516597, 40.86394065090267702, 12.00000000000001066 ) ) ;
#820 = ADVANCED_FACE ( 'NONE', ( #7360 ), #12154, .F. ) ;
#821 = AXIS2_PLACEMENT_3D ( 'NONE', #7186, #2427, #43 ) ;
#822 = EDGE_CURVE ( 'NONE', #13988, #1469, #4075, .T. ) ;
#823 = EDGE_CURVE ( 'NONE', #235, #10036, #14913, .T. ) ;
#824 = CARTESIAN_POINT ( 'NONE',  ( -216.9711578880983893, 150.1110767499728240, 9.578254705571840333 ) ) ;
#825 = DIRECTION ( 'NONE',  ( -0.000000000000000000, -0.000000000000000000, -1.000000000000000000 ) ) ;
#826 = CARTESIAN_POINT ( 'NONE',  ( 0.3173508448886544486, 8.480771745766400471, 1.310872448937999035 ) ) ;
#827 = PRODUCT ( 'Cast Iron Frame Side Blocks x2', 'Cast Iron Frame Side Blocks x2', '', ( #6581 ) ) ;
#828 = VERTEX_POINT ( 'NONE', #6562 ) ;
#829 = FACE_OUTER_BOUND ( 'NONE', #8158, .T. ) ;
#830 = VERTEX_POINT ( 'NONE', #4242 ) ;
#831 = VERTEX_POINT ( 'NONE', #526 ) ;
#832 = DIRECTION ( 'NONE',  ( -0.000000000000000000, -1.000000000000000000, -0.000000000000000000 ) ) ;
#833 = PLANE ( 'NONE',  #7276 ) ;
#834 = DIRECTION ( 'NONE',  ( -0.000000000000000000, 0.000000000000000000, 1.000000000000000000 ) ) ;
#835 = CARTESIAN_POINT ( 'NONE',  ( -168.4340493060770427, 126.4566329172550070, 6.894248570768724882 ) ) ;
#836 = CARTESIAN_POINT ( 'NONE',  ( -222.5645123348796801, 148.4799522099133640, -2.927675643679180428 ) ) ;
#837 = VECTOR ( 'NONE', #9700, 1000.000000000000000 ) ;
#838 = DIRECTION ( 'NONE',  ( 1.000000000000000000, 0.000000000000000000, 0.000000000000000000 ) ) ;
#839 = EDGE_CURVE ( 'NONE', #6369, #8350, #8141, .T. ) ;
#840 = AXIS2_PLACEMENT_3D ( 'NONE', #12273, #3526, #37 ) ;
#841 = DIRECTION ( 'NONE',  ( 0.000000000000000000, -1.000000000000000000, 0.000000000000000000 ) ) ;
#842 = CIRCLE ( 'NONE', #12444, 1.499999999999997780 ) ;
#843 = DIRECTION ( 'NONE',  ( 0.000000000000000000, 0.000000000000000000, -1.000000000000000000 ) ) ;
#844 = FACE_BOUND ( 'NONE', #3836, .T. ) ;
#845 = DIRECTION ( 'NONE',  ( 1.000000000000000000, 0.000000000000000000, 0.000000000000000000 ) ) ;
#846 = ORIENTED_EDGE ( 'NONE', *, *, #12928, .T. ) ;
#847 = AXIS2_PLACEMENT_3D ( 'NONE', #10566, #8058, #12846 ) ;
#848 = ORIENTED_EDGE ( 'NONE', *, *, #6781, .T. ) ;
#849 = CARTESIAN_POINT ( 'NONE',  ( -174.2601771783465097, 116.0182102862799383, 1.243088744850515459 ) ) ;
#850 = CARTESIAN_POINT ( 'NONE',  ( -216.7144175016715337, 154.8588128942135143, 3.150775860475527601 ) ) ;
#852 = ORIENTED_EDGE ( 'NONE', *, *, #6243, .T. ) ;
#851 = CIRCLE ( 'NONE', #6656, 1.499999999999997780 ) ;
#853 = CARTESIAN_POINT ( 'NONE',  ( -210.7165899865938172, 151.5484195431892545, 2.500000000000000000 ) ) ;
#854 = DIRECTION ( 'NONE',  ( 1.000000000000000000, 2.751328491981765035E-32, -3.965082230804130220E-16 ) ) ;
#855 = EDGE_CURVE ( 'NONE', #8929, #14758, #8389, .T. ) ;
#856 = EDGE_CURVE ( 'NONE', #10437, #9262, #1951, .T. ) ;
#857 = LINE ( 'NONE', #5690, #11930 ) ;
#858 = VERTEX_POINT ( 'NONE', #6644 ) ;
#859 = EDGE_CURVE ( 'NONE', #14554, #9030, #3433, .T. ) ;
#860 = AXIS2_PLACEMENT_3D ( 'NONE', #12437, #4145, #5109 ) ;
#861 = ITEM_DEFINED_TRANSFORMATION ( 'NONE', 'NONE', #3491,  #12337 ) ;
#862 = ORIENTED_EDGE ( 'NONE', *, *, #15336, .F. ) ;
#863 = CARTESIAN_POINT ( 'NONE',  ( 198.5781842723177704, 29.07471546161169229, -6.884323831650920766 ) ) ;
#864 = ORIENTED_EDGE ( 'NONE', *, *, #15101, .T. ) ;
#865 = CYLINDRICAL_SURFACE ( 'NONE', #11752, 1.699999999999994849 ) ;
#866 = CARTESIAN_POINT ( 'NONE',  ( 0.000000000000000000, -2.381569860407202643, 1.375000000000004663 ) ) ;
#867 = CARTESIAN_POINT ( 'NONE',  ( -223.5869895076567957, 142.0744606454175312, 3.511683908622253991 ) ) ;
#868 = VERTEX_POINT ( 'NONE', #5283 ) ;
#869 = ORIENTED_EDGE ( 'NONE', *, *, #13066, .F. ) ;
#870 = DIRECTION ( 'NONE',  ( 0.000000000000000000, 0.000000000000000000, -1.000000000000000000 ) ) ;
#871 = CARTESIAN_POINT ( 'NONE',  ( 200.1062858801516597, 40.86394065090267702, 16.00000000000001421 ) ) ;
#872 = CIRCLE ( 'NONE', #11474, 3.500000000000003109 ) ;
#873 = VERTEX_POINT ( 'NONE', #10108 ) ;
#874 = CARTESIAN_POINT ( 'NONE',  ( 51.39999999999999858, 0.000000000000000000, 0.000000000000000000 ) ) ;
#875 = DIRECTION ( 'NONE',  ( 1.000000000000000000, 0.000000000000000000, 0.000000000000000000 ) ) ;
#876 = CARTESIAN_POINT ( 'NONE',  ( 200.1062858801516597, 40.86394065090267702, 5.000000000000000000 ) ) ;
#877 = CARTESIAN_POINT ( 'NONE',  ( -61.94838851346079167, -179.3058001507315566, 84.88378295107887084 ) ) ;
#878 = VECTOR ( 'NONE', #7399, 1000.000000000000000 ) ;
#879 = DIRECTION ( 'NONE',  ( -0.000000000000000000, 0.000000000000000000, -1.000000000000000000 ) ) ;
#880 = ORIENTED_EDGE ( 'NONE', *, *, #9050, .T. ) ;
#881 = ADVANCED_FACE ( 'NONE', ( #4803 ), #11148, .T. ) ;
#882 = FACE_OUTER_BOUND ( 'NONE', #8952, .T. ) ;
#883 = CARTESIAN_POINT ( 'NONE',  ( -31.27399788034579586, 48.72489408690345414, 10.00000000000000178 ) ) ;
#884 = CARTESIAN_POINT ( 'NONE',  ( 184.0000000000000568, 15.53993994372673626, 47.49999999999997868 ) ) ;
#885 = ORIENTED_EDGE ( 'NONE', *, *, #8221, .F. ) ;
#886 = CARTESIAN_POINT ( 'NONE',  ( -191.3370974917540366, 126.0439545877573266, -0.4555467707853441128 ) ) ;
#887 = CARTESIAN_POINT ( 'NONE',  ( 190.6753907620029054, 48.10438271498464502, -4.747728522856008659 ) ) ;
#888 = EDGE_LOOP ( 'NONE', ( #12867, #4817, #14342, #1072 ) ) ;
#889 = EDGE_CURVE ( 'NONE', #9525, #12618, #11656, .T. ) ;
#890 = TOROIDAL_SURFACE ( 'NONE', #14004, 1.000000000000000000, 0.5000000000000000000 ) ;
#891 = DIRECTION ( 'NONE',  ( 0.000000000000000000, 1.000000000000000000, 1.156482317317871725E-16 ) ) ;
#892 = DIRECTION ( 'NONE',  ( 1.000000000000000000, -2.751328491981765035E-32, 3.965082230804130220E-16 ) ) ;
#893 = AXIS2_PLACEMENT_3D ( 'NONE', #8643, #9908, #8719 ) ;
#894 = DIRECTION ( 'NONE',  ( 3.965082230804130220E-16, 1.090924371466202084E-47, 1.000000000000000000 ) ) ;
#895 = EDGE_CURVE ( 'NONE', #11510, #13090, #8296, .T. ) ;
#896 = ORIENTED_EDGE ( 'NONE', *, *, #6653, .T. ) ;
#897 = SURFACE_STYLE_FILL_AREA ( #8426 ) ;
#898 = CARTESIAN_POINT ( 'NONE',  ( 208.8119045081773777, 39.60750423734790360, -5.989029428842635561 ) ) ;
#899 = VERTEX_POINT ( 'NONE', #14266 ) ;
#900 = DIRECTION ( 'NONE',  ( -0.000000000000000000, -0.000000000000000000, -1.000000000000000000 ) ) ;
#901 = CARTESIAN_POINT ( 'NONE',  ( -185.2335129678179726, 125.0353967269121966, 9.577123744044223841 ) ) ;
#902 = DIRECTION ( 'NONE',  ( 0.000000000000000000, 0.000000000000000000, 1.000000000000000000 ) ) ;
#903 = DIRECTION ( 'NONE',  ( 0.000000000000000000, 0.000000000000000000, 1.000000000000000000 ) ) ;
#904 = AXIS2_PLACEMENT_3D ( 'NONE', #11636, #9194, #4125 ) ;
#905 = PLANE ( 'NONE',  #8362 ) ;
#906 = TOROIDAL_SURFACE ( 'NONE', #7237, 21.91351791792154202, 1.499999999999997113 ) ;
#907 = EDGE_LOOP ( 'NONE', ( #8993, #12549, #11670, #14820 ) ) ;
#908 = VERTEX_POINT ( 'NONE', #2036 ) ;
#909 = CARTESIAN_POINT ( 'NONE',  ( -152.2204635237962691, 107.8706385701098185, 9.623760898223435944 ) ) ;
#910 = CARTESIAN_POINT ( 'NONE',  ( 64.00000000000005684, 62.13993994372673768, 15.00000000000070166 ) ) ;
#911 = ADVANCED_FACE ( 'NONE', ( #11682 ), #8886, .F. ) ;
#912 = CARTESIAN_POINT ( 'NONE',  ( -35.99999999999995026, 62.13993994372673768, 15.00000000000139977 ) ) ;
#913 = CARTESIAN_POINT ( 'NONE',  ( -150.4086188282879277, 107.2728346664360259, 0.000000000000000000 ) ) ;
#914 = CARTESIAN_POINT ( 'NONE',  ( -221.3664521364747202, 150.6264651190829511, -2.887957967080375443 ) ) ;
#916 = EDGE_CURVE ( 'NONE', #14981, #2732, #12150, .T. ) ;
#915 = EDGE_CURVE ( 'NONE', #3320, #10463, #3385, .T. ) ;
#917 = EDGE_CURVE ( 'NONE', #11949, #9422, #12929, .T. ) ;
#918 = CARTESIAN_POINT ( 'NONE',  ( 190.0000000000000568, 15.53993994372673981, -2.500000000000071054 ) ) ;
#919 = CIRCLE ( 'NONE', #9009, 1.000000000000000888 ) ;
#920 = CYLINDRICAL_SURFACE ( 'NONE', #10681, 1.500000000000001332 ) ;
#921 = EDGE_CURVE ( 'NONE', #12187, #12589, #5102, .T. ) ;
#922 = CARTESIAN_POINT ( 'NONE',  ( -35.99999999999995026, 59.53993994372674337, 13.30000000000139870 ) ) ;
#923 = CARTESIAN_POINT ( 'NONE',  ( -76.00000000000001421, 16.03993994372673981, -7.458121719691109004E-14 ) ) ;
#924 = CARTESIAN_POINT ( 'NONE',  ( 0.02351960456805774966, -2.112255972321529285, 1.841465337348299869 ) ) ;
#925 = DIRECTION ( 'NONE',  ( -1.000000000000000000, -0.000000000000000000, -0.000000000000000000 ) ) ;
#926 = ORIENTED_EDGE ( 'NONE', *, *, #13201, .T. ) ;
#927 = VERTEX_POINT ( 'NONE', #8374 ) ;
#928 = PLANE ( 'NONE',  #9563 ) ;
#929 = CIRCLE ( 'NONE', #7000, 2.000000000000000000 ) ;
#930 = CARTESIAN_POINT ( 'NONE',  ( 0.000000000000000000, -6.928203230275514990, 4.000000000000058620 ) ) ;
#931 = DIRECTION ( 'NONE',  ( 1.000000000000000000, 0.000000000000000000, 0.000000000000000000 ) ) ;
#932 = FILL_AREA_STYLE ('',( #8154 ) ) ;
#933 = DIRECTION ( 'NONE',  ( -0.000000000000000000, -0.000000000000000000, 1.000000000000000000 ) ) ;
#934 = ADVANCED_FACE ( 'NONE', ( #11911 ), #13001, .T. ) ;
#935 = VERTEX_POINT ( 'NONE', #2196 ) ;
#936 = VECTOR ( 'NONE', #12404, 1000.000000000000000 ) ;
#937 = ORIENTED_EDGE ( 'NONE', *, *, #4830, .T. ) ;
#938 = EDGE_CURVE ( 'NONE', #2958, #9645, #5088, .T. ) ;
#939 = CARTESIAN_POINT ( 'NONE',  ( -63.50000000000002842, -179.8058001507315566, -51.45141194869119516 ) ) ;
#940 = ORIENTED_EDGE ( 'NONE', *, *, #1886, .F. ) ;
#941 = CARTESIAN_POINT ( 'NONE',  ( -108.0000000000000568, 64.53993994372673626, 20.00000000000000355 ) ) ;
#942 = CARTESIAN_POINT ( 'NONE',  ( 172.5293059057019889, 61.25683321636181233, 7.600000000000002309 ) ) ;
#943 = PLANE ( 'NONE',  #13809 ) ;
#944 = VERTEX_POINT ( 'NONE', #5832 ) ;
#945 = ORIENTED_EDGE ( 'NONE', *, *, #7328, .T. ) ;
#946 = DIRECTION ( 'NONE',  ( 0.000000000000000000, 0.000000000000000000, 1.000000000000000000 ) ) ;
#947 = LINE ( 'NONE', #141, #14146 ) ;
#948 = EDGE_CURVE ( 'NONE', #14543, #645, #2118, .T. ) ;
#949 = ORIENTED_EDGE ( 'NONE', *, *, #2798, .T. ) ;
#950 = VECTOR ( 'NONE', #5040, 1000.000000000000000 ) ;
#951 = DIRECTION ( 'NONE',  ( -2.897122145519000304E-15, 0.9902680687415702510, 0.1391731009600660485 ) ) ;
#952 = CIRCLE ( 'NONE', #13851, 0.5000000000000004441 ) ;
#953 = CIRCLE ( 'NONE', #1966, 3.500000000000003109 ) ;
#954 = DIRECTION ( 'NONE',  ( -0.000000000000000000, 1.000000000000000000, 1.156482317317871725E-16 ) ) ;
#955 = ORIENTED_EDGE ( 'NONE', *, *, #7157, .T. ) ;
#956 = VERTEX_POINT ( 'NONE', #3310 ) ;
#957 = CARTESIAN_POINT ( 'NONE',  ( 0.000000000000000000, 19.53993994372674337, 2.905405074819403421E-15 ) ) ;
#958 = ORIENTED_EDGE ( 'NONE', *, *, #14050, .F. ) ;
#959 = CARTESIAN_POINT ( 'NONE',  ( 64.00000000000005684, 64.53993994372673626, 16.70000000000069207 ) ) ;
#960 = AXIS2_PLACEMENT_3D ( 'NONE', #2650, #2411, #6129 ) ;
#961 = DIRECTION ( 'NONE',  ( 0.000000000000000000, 0.000000000000000000, 1.000000000000000000 ) ) ;
#962 = PLANE ( 'NONE',  #6800 ) ;
#963 = ORIENTED_EDGE ( 'NONE', *, *, #5376, .T. ) ;
#964 = CARTESIAN_POINT ( 'NONE',  ( -223.5232045190763301, 146.7623046726374980, -4.689260562946596878 ) ) ;
#965 = CARTESIAN_POINT ( 'NONE',  ( 198.8104769829885754, 49.54338459298288200, -5.250705761417654216 ) ) ;
#966 = ORIENTED_EDGE ( 'NONE', *, *, #12260, .T. ) ;
#967 = EDGE_CURVE ( 'NONE', #50, #4287, #14667, .T. ) ;
#968 = CARTESIAN_POINT ( 'NONE',  ( 194.0000000000000568, 26.39124795404934076, 0.000000000000000000 ) ) ;
#969 = CARTESIAN_POINT ( 'NONE',  ( 0.3167204509598372519, 5.377136764700148674, 6.686525924292801903 ) ) ;
#970 = CIRCLE ( 'NONE', #11577, 335.5619230110239641 ) ;
#971 = DIRECTION ( 'NONE',  ( 0.000000000000000000, -0.000000000000000000, 1.000000000000000000 ) ) ;
#972 = AXIS2_PLACEMENT_3D ( 'NONE', #4604, #14298, #2077 ) ;
#973 = VERTEX_POINT ( 'NONE', #9469 ) ;
#974 = CARTESIAN_POINT ( 'NONE',  ( -1.759810615610709617, 9.840298378705808702, -0.9892725615588873200 ) ) ;
#975 = CARTESIAN_POINT ( 'NONE',  ( 198.8872864542346974, 32.16591232847088122, -2.310211674251309688 ) ) ;
#976 = EDGE_LOOP ( 'NONE', ( #1480, #10214, #12873, #13520 ) ) ;
#977 = CARTESIAN_POINT ( 'NONE',  ( 71.96535645333923981, 38.79159067395544014, 7.600000000000002309 ) ) ;
#978 = CARTESIAN_POINT ( 'NONE',  ( -214.6152097961127367, 135.6358893629490581, -0.4555467707853336767 ) ) ;
#979 = VECTOR ( 'NONE', #3430, 1000.000000000000000 ) ;
#980 = LINE ( 'NONE', #14245, #1723 ) ;
#981 = CARTESIAN_POINT ( 'NONE',  ( -156.6477983077465410, 110.1970436846185066, 84.88378295107887084 ) ) ;
#982 = CIRCLE ( 'NONE', #8569, 1.499999999999994227 ) ;
#983 = CARTESIAN_POINT ( 'NONE',  ( 208.8060099514817978, 42.07246638764446089, -7.432400171711813996 ) ) ;
#984 = ADVANCED_FACE ( 'NONE', ( #6951, #7191 ), #3540, .T. ) ;
#985 = ORIENTED_EDGE ( 'NONE', *, *, #11407, .T. ) ;
#986 = EDGE_LOOP ( 'NONE', ( #15497, #15442, #9179, #14463 ) ) ;
#987 = FACE_OUTER_BOUND ( 'NONE', #2580, .T. ) ;
#988 = FACE_BOUND ( 'NONE', #7044, .T. ) ;
#989 = EDGE_CURVE ( 'NONE', #4028, #7962, #7888, .T. ) ;
#990 = LINE ( 'NONE', #10329, #3876 ) ;
#991 = LINE ( 'NONE', #2500, #12258 ) ;
#992 = CARTESIAN_POINT ( 'NONE',  ( -222.3946175953714999, 148.7843453047176467, -2.994737441843033476 ) ) ;
#993 = VECTOR ( 'NONE', #10687, 1000.000000000000000 ) ;
#994 = AXIS2_PLACEMENT_3D ( 'NONE', #12797, #10367, #1984 ) ;
#995 = DIRECTION ( 'NONE',  ( 0.000000000000000000, 0.000000000000000000, 1.000000000000000000 ) ) ;
#996 = DIRECTION ( 'NONE',  ( 0.000000000000000000, 0.000000000000000000, -1.000000000000000000 ) ) ;
#997 = CARTESIAN_POINT ( 'NONE',  ( 176.0293059057019889, 61.25683321636181233, 7.600000000000002309 ) ) ;
#998 = EDGE_CURVE ( 'NONE', #9262, #11923, #11758, .T. ) ;
#999 = PLANE ( 'NONE',  #14722 ) ;
#1000 = CARTESIAN_POINT ( 'NONE',  ( -206.0179204244930702, 148.9258921110169638, 2.500000000000000000 ) ) ;
#1001 = DIRECTION ( 'NONE',  ( -1.000000000000000000, 0.000000000000000000, 0.000000000000000000 ) ) ;
#1002 = CIRCLE ( 'NONE', #10862, 1.499999999999994449 ) ;
#1003 = DIRECTION ( 'NONE',  ( 0.000000000000000000, 0.1391731009600592484, 0.9902680687415712502 ) ) ;
#1004 = ORIENTED_EDGE ( 'NONE', *, *, #2372, .T. ) ;
#1005 = AXIS2_PLACEMENT_3D ( 'NONE', #12927, #3078, #15361 ) ;
#1006 = EDGE_CURVE ( 'NONE', #4775, #10379, #5752, .T. ) ;
#1007 = AXIS2_PLACEMENT_3D ( 'NONE', #2898, #5252, #7561 ) ;
#1008 = CARTESIAN_POINT ( 'NONE',  ( -63.50000000000002842, -179.8058001507315566, 84.88378295107887084 ) ) ;
#1009 = ORIENTED_EDGE ( 'NONE', *, *, #8860, .T. ) ;
#1010 = DIRECTION ( 'NONE',  ( -1.000000000000000000, 0.000000000000000000, 0.000000000000000000 ) ) ;
#1011 = CARTESIAN_POINT ( 'NONE',  ( -216.7032046242510148, 154.8780296845847033, 2.891444798692482721 ) ) ;
#1012 = CARTESIAN_POINT ( 'NONE',  ( -6.657678965418798693E-16, -7.321656987762860780, 3.318518101603048276 ) ) ;
#1013 = CARTESIAN_POINT ( 'NONE',  ( -193.7200834347810599, 142.0619459586758921, 2.500000000000000000 ) ) ;
#1014 = CARTESIAN_POINT ( 'NONE',  ( 190.5000000000000568, 17.53993994372674692, -17.50000000000002487 ) ) ;
#1015 = EDGE_CURVE ( 'NONE', #14712, #13022, #15364, .T. ) ;
#1016 = ADVANCED_FACE ( 'NONE', ( #2509 ), #2326, .T. ) ;
#1017 = CIRCLE ( 'NONE', #6335, 3.500000000000003109 ) ;
#1018 = EDGE_LOOP ( 'NONE', ( #2531, #11475, #6093, #963 ) ) ;
#1019 = AXIS2_PLACEMENT_3D ( 'NONE', #10169, #11272, #4150 ) ;
#1020 = ORIENTED_EDGE ( 'NONE', *, *, #14970, .T. ) ;
#1021 = CARTESIAN_POINT ( 'NONE',  ( 192.9079700310636269, 50.30505391962363149, -5.011923969639807019 ) ) ;
#1022 = PRESENTATION_STYLE_ASSIGNMENT (( #8312 ) ) ;
#1023 = ORIENTED_EDGE ( 'NONE', *, *, #4835, .T. ) ;
#1024 = DIRECTION ( 'NONE',  ( -0.000000000000000000, 1.000000000000000000, -0.000000000000000000 ) ) ;
#1025 = EDGE_CURVE ( 'NONE', #9103, #13250, #7487, .T. ) ;
#1026 = EDGE_CURVE ( 'NONE', #8395, #4264, #11155, .T. ) ;
#1027 = DIRECTION ( 'NONE',  ( -0.000000000000000000, -0.000000000000000000, 1.000000000000000000 ) ) ;
#1028 = EDGE_CURVE ( 'NONE', #2448, #379, #6375, .T. ) ;
#1029 = DIRECTION ( 'NONE',  ( 1.000000000000000000, 0.000000000000000000, 0.000000000000000000 ) ) ;
#1030 = ORIENTED_EDGE ( 'NONE', *, *, #12016, .T. ) ;
#1031 = EDGE_LOOP ( 'NONE', ( #14134, #3474, #14069, #6884 ) ) ;
#1032 = DIRECTION ( 'NONE',  ( 0.8660254037844385966, 0.5000000000000001110, -0.000000000000000000 ) ) ;
#1033 = LINE ( 'NONE', #4508, #9633 ) ;
#1034 = AXIS2_PLACEMENT_3D ( 'NONE', #635, #3025, #4190 ) ;
#1035 = ORIENTED_EDGE ( 'NONE', *, *, #1489, .T. ) ;
#1036 = CARTESIAN_POINT ( 'NONE',  ( -152.2117530991619958, 106.6622082107205216, 9.223488592771907690 ) ) ;
#1037 = CARTESIAN_POINT ( 'NONE',  ( -156.6477983077465410, 110.1970436846185066, -5.000000000000000000 ) ) ;
#1038 = CIRCLE ( 'NONE', #11412, 4.499999999999950262 ) ;
#1039 = LINE ( 'NONE', #8549, #12659 ) ;
#1040 = VECTOR ( 'NONE', #1882, 1000.000000000000227 ) ;
#1041 = ADVANCED_FACE ( 'NONE', ( #2431 ), #2744, .F. ) ;
#1042 = EDGE_LOOP ( 'NONE', ( #11606, #15270 ) ) ;
#1043 = CARTESIAN_POINT ( 'NONE',  ( 50.57199999999998852, 0.000000000000000000, 0.000000000000000000 ) ) ;
#1044 = CIRCLE ( 'NONE', #5333, 7.499999999999999112 ) ;
#1045 = ORIENTED_EDGE ( 'NONE', *, *, #6433, .F. ) ;
#1046 = CARTESIAN_POINT ( 'NONE',  ( -135.3034657297974093, 107.4444500778096483, 5.000000000000000000 ) ) ;
#1047 = B_SPLINE_CURVE_WITH_KNOTS ( 'NONE', 3,
 ( #2845, #7667, #5054, #3868, #13558, #8927 ),
 .UNSPECIFIED., .F., .F.,
 ( 4, 2, 4 ),
 ( 0.008378281255485226300, 0.009182315005745945308, 0.009986348756006662580 ),
 .UNSPECIFIED. ) ;
#1048 = LINE ( 'NONE', #6988, #13883 ) ;
#1049 = CARTESIAN_POINT ( 'NONE',  ( -76.00000000000001421, 15.03993994372673981, -3.075184203610571654 ) ) ;
#1050 = ORIENTED_EDGE ( 'NONE', *, *, #11057, .F. ) ;
#1051 = CARTESIAN_POINT ( 'NONE',  ( -181.1480734112017501, 126.1383063644306617, -5.230826428279600648 ) ) ;
#1052 = CARTESIAN_POINT ( 'NONE',  ( 207.1558710170397433, 35.63411313097393673, -9.376170956558697256 ) ) ;
#1053 = EDGE_LOOP ( 'NONE', ( #1556, #9864 ) ) ;
#1054 = AXIS2_PLACEMENT_3D ( 'NONE', #1853, #3198, #15183 ) ;
#1055 = CARTESIAN_POINT ( 'NONE',  ( 190.5000000000000568, 15.03993994372673981, -3.075184203610571654 ) ) ;
#1056 = FACE_OUTER_BOUND ( 'NONE', #9716, .T. ) ;
#1057 = VECTOR ( 'NONE', #10570, 1000.000000000000000 ) ;
#1058 = DIRECTION ( 'NONE',  ( 1.000000000000000000, 0.000000000000000000, 0.000000000000000000 ) ) ;
#1059 = ADVANCED_FACE ( 'NONE', ( #12139 ), #2593, .T. ) ;
#1060 = ORIENTED_EDGE ( 'NONE', *, *, #7722, .T. ) ;
#1061 =( LENGTH_UNIT ( ) NAMED_UNIT ( * ) SI_UNIT ( .MILLI., .METRE. ) );
#1062 = CARTESIAN_POINT ( 'NONE',  ( 178.0000000000000853, -178.8058001507315566, 65.31842631998698323 ) ) ;
#1063 = CARTESIAN_POINT ( 'NONE',  ( 201.2541767070109984, 32.14103196098812987, -5.186035738131804962 ) ) ;
#1064 = EDGE_LOOP ( 'NONE', ( #7124, #5619, #4807, #15346, #2670, #14276 ) ) ;
#1065 = LINE ( 'NONE', #10870, #11730 ) ;
#1066 = CARTESIAN_POINT ( 'NONE',  ( -213.9961813491638623, 134.6717504882919911, 1.515400478619087776 ) ) ;
#1067 = DIRECTION ( 'NONE',  ( 0.000000000000000000, 0.000000000000000000, 1.000000000000000000 ) ) ;
#1068 = DIRECTION ( 'NONE',  ( 0.000000000000000000, 0.000000000000000000, 1.000000000000000000 ) ) ;
#1069 = AXIS2_PLACEMENT_3D ( 'NONE', #6183, #9807, #13259 ) ;
#1070 = LINE ( 'NONE', #10710, #2815 ) ;
#1071 = VERTEX_POINT ( 'NONE', #6301 ) ;
#1072 = ORIENTED_EDGE ( 'NONE', *, *, #11053, .F. ) ;
#1073 = CARTESIAN_POINT ( 'NONE',  ( -217.6653619995784652, 138.6635820529667740, 2.431555724346871283 ) ) ;
#1074 = CARTESIAN_POINT ( 'NONE',  ( 0.7145311798163189732, 4.618802153516981868, -7.999999999999979572 ) ) ;
#1075 = CYLINDRICAL_SURFACE ( 'NONE', #12938, 1.699999999999991518 ) ;
#1076 = DIRECTION ( 'NONE',  ( 0.000000000000000000, 0.000000000000000000, -1.000000000000000000 ) ) ;
#1077 = EDGE_CURVE ( 'NONE', #10971, #14401, #8747, .T. ) ;
#1078 = CARTESIAN_POINT ( 'NONE',  ( -219.3877568461323619, 150.1024971847152756, -4.823803736792959818 ) ) ;
#1079 = CARTESIAN_POINT ( 'NONE',  ( -223.4717893243274602, 142.3106348291761662, 4.713848895078025514 ) ) ;
#1080 = VECTOR ( 'NONE', #3010, 1000.000000000000000 ) ;
#1081 = FACE_OUTER_BOUND ( 'NONE', #6812, .T. ) ;
#1082 = CARTESIAN_POINT ( 'NONE',  ( 0.000000000000000000, 0.000000000000000000, 0.000000000000000000 ) ) ;
#1083 = LINE ( 'NONE', #6073, #2781 ) ;
#1084 = CARTESIAN_POINT ( 'NONE',  ( -156.6477983077465410, 110.1970436846185066, 5.000000000000004441 ) ) ;
#1085 = CARTESIAN_POINT ( 'NONE',  ( -34.79899788034579444, 48.72489408690345414, 7.600000000000002309 ) ) ;
#1086 = EDGE_LOOP ( 'NONE', ( #8415, #5150, #14250, #3362 ) ) ;
#1087 = EDGE_CURVE ( 'NONE', #6095, #12779, #3924, .T. ) ;
#1088 = SHAPE_REPRESENTATION_RELATIONSHIP ( 'NONE' , 'NONE' ,  #5419, #10743 ) ;
#1089 = ORIENTED_EDGE ( 'NONE', *, *, #5398, .F. ) ;
#1090 = DIRECTION ( 'NONE',  ( 0.000000000000000000, -1.000000000000000000, -2.731481088613025116E-16 ) ) ;
#1091 = AXIS2_PLACEMENT_3D ( 'NONE', #5904, #14335, #10721 ) ;
#1092 = DIRECTION ( 'NONE',  ( -0.000000000000000000, -0.000000000000000000, -1.000000000000000000 ) ) ;
#1093 = FACE_OUTER_BOUND ( 'NONE', #8112, .T. ) ;
#1094 = CARTESIAN_POINT ( 'NONE',  ( -218.4488137430494419, 155.8538722928748541, 3.478855109783925315 ) ) ;
#1095 = VECTOR ( 'NONE', #6395, 1000.000000000000000 ) ;
#1096 = EDGE_LOOP ( 'NONE', ( #7071, #14748 ) ) ;
#1097 = EDGE_CURVE ( 'NONE', #8873, #8651, #1552, .T. ) ;
#1098 = VERTEX_POINT ( 'NONE', #10967 ) ;
#1099 = AXIS2_PLACEMENT_3D ( 'NONE', #524, #761, #9079 ) ;
#1100 = CARTESIAN_POINT ( 'NONE',  ( 208.8060099514817978, 42.07246638764446089, -7.432400171711813996 ) ) ;
#1101 = CARTESIAN_POINT ( 'NONE',  ( 190.0000000000000568, 13.40307322461932493, -2.295403246091865412 ) ) ;
#1102 = EDGE_LOOP ( 'NONE', ( #10073, #2655 ) ) ;
#1103 = CARTESIAN_POINT ( 'NONE',  ( 175.9483885134608272, 15.03993994372673981, -3.075184203610571654 ) ) ;
#1104 = AXIS2_PLACEMENT_3D ( 'NONE', #6378, #3194, #15329 ) ;
#1105 = CARTESIAN_POINT ( 'NONE',  ( -224.7518895393548348, 144.5609225879004498, 7.521475632127809341 ) ) ;
#1106 = EDGE_LOOP ( 'NONE', ( #4528, #9454, #14687, #11346 ) ) ;
#1107 = ORIENTED_EDGE ( 'NONE', *, *, #3537, .T. ) ;
#1108 = LINE ( 'NONE', #1260, #15580 ) ;
#1109 = LINE ( 'NONE', #3563, #4063 ) ;
#1110 = ORIENTED_EDGE ( 'NONE', *, *, #1281, .F. ) ;
#1111 = CYLINDRICAL_SURFACE ( 'NONE', #6828, 4.499999999999950262 ) ;
#1112 = AXIS2_PLACEMENT_3D ( 'NONE', #7296, #5521, #12474 ) ;
#1113 = FACE_OUTER_BOUND ( 'NONE', #15215, .T. ) ;
#1114 = EDGE_CURVE ( 'NONE', #6055, #3552, #2548, .T. ) ;
#1116 = ADVANCED_FACE ( 'NONE', ( #8520, #13469, #274 ), #7343, .F. ) ;
#1115 = EDGE_CURVE ( 'NONE', #10711, #12769, #14133, .T. ) ;
#1117 = ORIENTED_EDGE ( 'NONE', *, *, #218, .F. ) ;
#1118 = LINE ( 'NONE', #14294, #8578 ) ;
#1119 = DIRECTION ( 'NONE',  ( 3.965082230804130220E-16, 0.000000000000000000, 1.000000000000000000 ) ) ;
#1120 = ORIENTED_EDGE ( 'NONE', *, *, #3798, .F. ) ;
#1121 = DIRECTION ( 'NONE',  ( 1.000000000000000000, 0.000000000000000000, 0.000000000000000000 ) ) ;
#1122 = AXIS2_PLACEMENT_3D ( 'NONE', #11812, #7243, #8431 ) ;
#1123 = CARTESIAN_POINT ( 'NONE',  ( 51.39999999999999858, 0.000000000000000000, 4.172000000000013920 ) ) ;
#1124 = DIRECTION ( 'NONE',  ( 0.000000000000000000, 1.000000000000000000, 6.938893903907227145E-17 ) ) ;
#1125 = EDGE_LOOP ( 'NONE', ( #7007, #5807 ) ) ;
#1126 = VERTEX_POINT ( 'NONE', #4961 ) ;
#1127 = CARTESIAN_POINT ( 'NONE',  ( -216.9311889273521672, 150.1826874172201656, -4.640918829492440167 ) ) ;
#1128 = CARTESIAN_POINT ( 'NONE',  ( 211.8745662956760896, 42.53653439883859022, -6.011979689023970508 ) ) ;
#1129 = EDGE_LOOP ( 'NONE', ( #6452, #6459, #7636, #5771, #1089 ) ) ;
#1130 = CARTESIAN_POINT ( 'NONE',  ( 166.9217645774054120, 62.57671370024034729, -0.9107274384406883749 ) ) ;
#1131 = CARTESIAN_POINT ( 'NONE',  ( 0.06809871960542698832, 6.146186931204399961, 5.354491962338134847 ) ) ;
#1132 = DIRECTION ( 'NONE',  ( 1.000000000000000000, 0.000000000000000000, 0.000000000000000000 ) ) ;
#1133 = VECTOR ( 'NONE', #9502, 1000.000000000000000 ) ;
#1134 = ORIENTED_EDGE ( 'NONE', *, *, #3215, .F. ) ;
#1135 = FACE_OUTER_BOUND ( 'NONE', #5191, .T. ) ;
#1136 = CARTESIAN_POINT ( 'NONE',  ( 198.8634854004546071, 49.55149448133588663, -6.680369717582868461 ) ) ;
#1137 = VERTEX_POINT ( 'NONE', #9938 ) ;
#1138 = PLANE ( 'NONE',  #4834 ) ;
#1139 = FACE_OUTER_BOUND ( 'NONE', #12303, .T. ) ;
#1140 = CARTESIAN_POINT ( 'NONE',  ( -225.7548303624724610, 142.7639966680278576, 1.446957622915672204 ) ) ;
#1141 = B_SPLINE_CURVE_WITH_KNOTS ( 'NONE', 3,
 ( #9451, #1143, #4386, #9217, #6853, #826, #13051, #2254 ),
 .UNSPECIFIED., .F., .F.,
 ( 4, 2, 2, 4 ),
 ( 0.004673709593152155714, 0.005837709341827646871, 0.007001709090503138028, 0.009329708587854120341 ),
 .UNSPECIFIED. ) ;
#1142 = CYLINDRICAL_SURFACE ( 'NONE', #13573, 1.000000000000000888 ) ;
#1143 = CARTESIAN_POINT ( 'NONE',  ( -5.065680541054341600E-15, 7.124194613927618214, 3.660532965668821692 ) ) ;
#1144 = CARTESIAN_POINT ( 'NONE',  ( -203.7296541848517109, 135.3294987143146955, 9.577123744044227394 ) ) ;
#1145 = CARTESIAN_POINT ( 'NONE',  ( 208.8051451104704768, 39.65587490144260840, -4.559632177755815086 ) ) ;
#1146 = AXIS2_PLACEMENT_3D ( 'NONE', #5074, #9818, #3958 ) ;
#1147 = ORIENTED_EDGE ( 'NONE', *, *, #3050, .T. ) ;
#1148 = ORIENTED_EDGE ( 'NONE', *, *, #17, .F. ) ;
#1149 = CARTESIAN_POINT ( 'NONE',  ( -76.00000000000001421, -179.8058001507315566, -17.19066787724516843 ) ) ;
#1150 = FACE_BOUND ( 'NONE', #2621, .T. ) ;
#1151 = ADVANCED_FACE ( 'NONE', ( #13538 ), #13394, .F. ) ;
#1152 = DIRECTION ( 'NONE',  ( 1.000000000000000000, 0.000000000000000000, 0.000000000000000000 ) ) ;
#1153 = DIRECTION ( 'NONE',  ( 0.000000000000000000, 0.000000000000000000, 1.000000000000000000 ) ) ;
#1154 = DIRECTION ( 'NONE',  ( 0.000000000000000000, 1.000000000000000000, 0.000000000000000000 ) ) ;
#1155 = CARTESIAN_POINT ( 'NONE',  ( -218.9545055651059045, 150.9247396209540568, 9.391049919365073606 ) ) ;
#1156 = CARTESIAN_POINT ( 'NONE',  ( 178.0000000000000853, 15.03993994372673804, 38.07518420361041933 ) ) ;
#1157 = CARTESIAN_POINT ( 'NONE',  ( -63.50000000000002842, 14.97035339324670744, 37.58005016923963382 ) ) ;
#1158 = CARTESIAN_POINT ( 'NONE',  ( -157.6477983077465694, 110.0680497146841077, 9.367218745794341217 ) ) ;
#1159 = DIRECTION ( 'NONE',  ( 0.000000000000000000, -0.000000000000000000, -1.000000000000000000 ) ) ;
#1160 = DIRECTION ( 'NONE',  ( 0.000000000000000000, 0.000000000000000000, 1.000000000000000000 ) ) ;
#1161 = VERTEX_POINT ( 'NONE', #5190 ) ;
#1162 = ORIENTED_EDGE ( 'NONE', *, *, #10778, .F. ) ;
#1163 = EDGE_CURVE ( 'NONE', #4062, #3314, #3306, .T. ) ;
#1164 = DIRECTION ( 'NONE',  ( -0.000000000000000000, 1.000000000000000000, -0.000000000000000000 ) ) ;
#1165 = CARTESIAN_POINT ( 'NONE',  ( 175.9483885134608272, 15.03993994372673981, -2.575184203610571654 ) ) ;
#1166 = SURFACE_STYLE_USAGE ( .BOTH. , #11997 ) ;
#1167 = FACE_BOUND ( 'NONE', #3663, .T. ) ;
#1168 = CARTESIAN_POINT ( 'NONE',  ( 51.07686401294030532, 368.7106150007013525, 10.00000000000000178 ) ) ;
#1169 = DIRECTION ( 'NONE',  ( -0.000000000000000000, 1.000000000000000000, -0.000000000000000000 ) ) ;
#1170 = ORIENTED_EDGE ( 'NONE', *, *, #14936, .F. ) ;
#1171 = ORIENTED_EDGE ( 'NONE', *, *, #5302, .T. ) ;
#1172 = CARTESIAN_POINT ( 'NONE',  ( 205.4931693814993139, 33.91842896272902408, -6.501828201457912293 ) ) ;
#1173 = CARTESIAN_POINT ( 'NONE',  ( 178.0000000000000853, -178.8058001507315566, -17.69066787724516843 ) ) ;
#1174 = ORIENTED_EDGE ( 'NONE', *, *, #12928, .F. ) ;
#1175 = VECTOR ( 'NONE', #10098, 1000.000000000000000 ) ;
#1176 = CARTESIAN_POINT ( 'NONE',  ( -224.5448265106511769, 144.9319085071302879, 3.590746859383691536 ) ) ;
#1177 = ORIENTED_EDGE ( 'NONE', *, *, #7018, .T. ) ;
#1178 = VERTEX_POINT ( 'NONE', #10894 ) ;
#1179 = CARTESIAN_POINT ( 'NONE',  ( -34.79899788034579444, 48.72489408690345414, 5.000000000000000000 ) ) ;
#1180 = CARTESIAN_POINT ( 'NONE',  ( 119.0806775638430253, 45.00321902537314145, 10.00000000000000178 ) ) ;
#1181 = EDGE_CURVE ( 'NONE', #13859, #5228, #502, .T. ) ;
#1182 = EDGE_LOOP ( 'NONE', ( #11077, #12409, #5539, #8357 ) ) ;
#1183 = CARTESIAN_POINT ( 'NONE',  ( 190.5000000000000853, 17.53993994372673271, 52.49999999999997868 ) ) ;
#1184 = DIRECTION ( 'NONE',  ( 0.000000000000000000, 1.000000000000000000, 0.000000000000000000 ) ) ;
#1185 = DIRECTION ( 'NONE',  ( -0.000000000000000000, -0.000000000000000000, 1.000000000000000000 ) ) ;
#1186 = ORIENTED_EDGE ( 'NONE', *, *, #3880, .F. ) ;
#1187 = EDGE_CURVE ( 'NONE', #227, #1631, #1934, .T. ) ;
#1188 = CARTESIAN_POINT ( 'NONE',  ( -63.50000000000002842, 17.53993994372673626, 52.49999999999997868 ) ) ;
#1189 = CIRCLE ( 'NONE', #6262, 3.500000000000003109 ) ;
#1190 = CYLINDRICAL_SURFACE ( 'NONE', #4296, 1.499999999999994449 ) ;
#1191 = CARTESIAN_POINT ( 'NONE',  ( -150.9178095878665715, 108.1541761000636086, -4.963902819945232636 ) ) ;
#1192 = ORIENTED_EDGE ( 'NONE', *, *, #9834, .F. ) ;
#1193 = ORIENTED_EDGE ( 'NONE', *, *, #2572, .F. ) ;
#1194 = CARTESIAN_POINT ( 'NONE',  ( -202.8891874331996519, 144.7632710727894505, -2.963320117457099112 ) ) ;
#1195 = CARTESIAN_POINT ( 'NONE',  ( 211.8802283582561472, 39.29745248741442509, -3.136047433260559902 ) ) ;
#1196 = CIRCLE ( 'NONE', #10531, 1.700000000000007061 ) ;
#1197 = ORIENTED_EDGE ( 'NONE', *, *, #13835, .T. ) ;
#1198 = EDGE_CURVE ( 'NONE', #5867, #10763, #5282, .T. ) ;
#1199 = DIRECTION ( 'NONE',  ( 0.000000000000000000, 0.000000000000000000, 1.000000000000000000 ) ) ;
#1200 = DIRECTION ( 'NONE',  ( 0.2728218852358202384, -0.9620645606903794889, 8.659560562354905741E-17 ) ) ;
#1201 = ADVANCED_FACE ( 'NONE', ( #14881 ), #9062, .F. ) ;
#1202 = CARTESIAN_POINT ( 'NONE',  ( 190.5000000000000853, 15.03993994372673804, 38.07518420361041933 ) ) ;
#1203 = AXIS2_PLACEMENT_3D ( 'NONE', #3408, #15232, #11541 ) ;
#1204 = ORIENTED_EDGE ( 'NONE', *, *, #5302, .F. ) ;
#1205 = AXIS2_PLACEMENT_3D ( 'NONE', #14240, #7161, #12319 ) ;
#1206 = AXIS2_PLACEMENT_3D ( 'NONE', #7566, #6150, #9937 ) ;
#1207 = SURFACE_STYLE_USAGE ( .BOTH. , #2168 ) ;
#1208 = CARTESIAN_POINT ( 'NONE',  ( 198.8863654052626657, 49.55881746625484396, -3.681704842056328086 ) ) ;
#1209 = ORIENTED_EDGE ( 'NONE', *, *, #9778, .T. ) ;
#1210 = LINE ( 'NONE', #12263, #6859 ) ;
#1211 = DIRECTION ( 'NONE',  ( -1.000000000000000000, 0.000000000000000000, 0.000000000000000000 ) ) ;
#1212 = CARTESIAN_POINT ( 'NONE',  ( -191.4964613557999655, 125.7493975051623352, 3.478895870929489043 ) ) ;
#1213 = DIRECTION ( 'NONE',  ( 0.000000000000000000, 0.000000000000000000, 1.000000000000000000 ) ) ;
#1214 = VERTEX_POINT ( 'NONE', #4076 ) ;
#1215 = CARTESIAN_POINT ( 'NONE',  ( -210.0240857098682454, 141.7683007401625446, 10.16010209732750624 ) ) ;
#1216 = CARTESIAN_POINT ( 'NONE',  ( 201.2541767070109984, 32.14103196098812987, -5.186035738131804962 ) ) ;
#1217 = ADVANCED_FACE ( 'NONE', ( #2828 ), #7827, .T. ) ;
#1218 = AXIS2_PLACEMENT_3D ( 'NONE', #1179, #3479, #13179 ) ;
#1219 = ORIENTED_EDGE ( 'NONE', *, *, #14249, .T. ) ;
#1220 = ADVANCED_FACE ( 'NONE', ( #10165 ), #15113, .F. ) ;
#1221 = CIRCLE ( 'NONE', #8799, 1.499999999999994449 ) ;
#1222 = ORIENTED_EDGE ( 'NONE', *, *, #4363, .T. ) ;
#1223 = DIRECTION ( 'NONE',  ( 1.000000000000000000, 0.000000000000000000, 0.000000000000000000 ) ) ;
#1224 = CARTESIAN_POINT ( 'NONE',  ( 0.4988340113715718505, 3.871605243926934392, -7.999999999999981348 ) ) ;
#1225 = AXIS2_PLACEMENT_3D ( 'NONE', #14550, #2571, #8505 ) ;
#1226 = DIRECTION ( 'NONE',  ( -0.000000000000000000, -0.000000000000000000, 1.000000000000000000 ) ) ;
#1227 = FACE_OUTER_BOUND ( 'NONE', #14901, .T. ) ;
#1228 = CARTESIAN_POINT ( 'NONE',  ( -224.5811800873044604, 144.8667753680074384, 1.831365460742872209 ) ) ;
#1229 = CARTESIAN_POINT ( 'NONE',  ( 178.0000000000000853, 15.53993994372673981, -3.075184203610571654 ) ) ;
#1230 = CIRCLE ( 'NONE', #10074, 0.5000000000000001110 ) ;
#1231 = DIRECTION ( 'NONE',  ( -0.2258817899775119320, -0.9741547192086866813, 0.000000000000000000 ) ) ;
#1232 = FACE_OUTER_BOUND ( 'NONE', #10027, .T. ) ;
#1233 = VECTOR ( 'NONE', #806, 1000.000000000000114 ) ;
#1234 = EDGE_CURVE ( 'NONE', #4804, #2746, #9270, .T. ) ;
#1235 = CARTESIAN_POINT ( 'NONE',  ( -76.50000000000001421, 16.03993994372673981, 9.617930870223348805 ) ) ;
#1236 = DIRECTION ( 'NONE',  ( 0.000000000000000000, 4.956352788505162775E-17, -1.000000000000000000 ) ) ;
#1237 = ORIENTED_EDGE ( 'NONE', *, *, #7297, .T. ) ;
#1238 = EDGE_LOOP ( 'NONE', ( #9544, #15230, #13995, #7422 ) ) ;
#1239 = CIRCLE ( 'NONE', #6307, 3.500000000000001332 ) ;
#1240 = DIRECTION ( 'NONE',  ( -1.000000000000000000, 0.000000000000000000, 0.000000000000000000 ) ) ;
#1241 = CARTESIAN_POINT ( 'NONE',  ( -64.00000000000002842, 14.97035339324670922, -2.580050169239785696 ) ) ;
#1242 = AXIS2_PLACEMENT_3D ( 'NONE', #12493, #11401, #7940 ) ;
#1243 = LINE ( 'NONE', #3465, #6640 ) ;
#1244 = CIRCLE ( 'NONE', #10080, 1.499999999999997780 ) ;
#1245 = DIRECTION ( 'NONE',  ( -0.000000000000000000, 1.000000000000000000, 1.156482317317871725E-16 ) ) ;
#1246 = PLANE ( 'NONE',  #7999 ) ;
#1247 = CIRCLE ( 'NONE', #3275, 1.000000000000000888 ) ;
#1248 = CARTESIAN_POINT ( 'NONE',  ( 14.00000000000004086, 64.53993994372673626, 15.00000000000104983 ) ) ;
#1249 = CARTESIAN_POINT ( 'NONE',  ( -61.94838851346079167, -178.8058001507315566, 52.19066787724494816 ) ) ;
#1250 = ORIENTED_EDGE ( 'NONE', *, *, #13676, .T. ) ;
#1251 = EDGE_CURVE ( 'NONE', #9250, #11935, #13867, .T. ) ;
#1252 = AXIS2_PLACEMENT_3D ( 'NONE', #10138, #10216, #6512 ) ;
#1253 = AXIS2_PLACEMENT_3D ( 'NONE', #3458, #10965, #5829 ) ;
#1254 = ORIENTED_EDGE ( 'NONE', *, *, #14681, .F. ) ;
#1255 = CARTESIAN_POINT ( 'NONE',  ( 198.9643688939780191, 32.15902683440354082, -3.879216492611309519 ) ) ;
#1256 = CARTESIAN_POINT ( 'NONE',  ( 170.8293059057019718, 61.25683321636181233, 10.00000000000000178 ) ) ;
#1257 = ORIENTED_EDGE ( 'NONE', *, *, #4917, .T. ) ;
#1258 = CARTESIAN_POINT ( 'NONE',  ( -221.2417723974670878, 146.6801937162670697, 9.651042165284529517 ) ) ;
#1259 = EDGE_LOOP ( 'NONE', ( #5459, #10454, #4600, #3411 ) ) ;
#1260 = CARTESIAN_POINT ( 'NONE',  ( -35.99999999999995026, 64.53993994372673626, 11.50000000000139622 ) ) ;
#1261 = CARTESIAN_POINT ( 'NONE',  ( 192.9009781015629699, 50.32399521507879570, -6.439879401016198379 ) ) ;
#1262 = ORIENTED_EDGE ( 'NONE', *, *, #6535, .T. ) ;
#1263 = LINE ( 'NONE', #14523, #2893 ) ;
#1264 = CARTESIAN_POINT ( 'NONE',  ( -76.50000000000001421, -179.3058001507315566, -51.45141194869120227 ) ) ;
#1265 = AXIS2_PLACEMENT_3D ( 'NONE', #8938, #301, #14754 ) ;
#1266 = AXIS2_PLACEMENT_3D ( 'NONE', #9362, #6996, #2090 ) ;
#1267 = EDGE_CURVE ( 'NONE', #3320, #3389, #13855, .T. ) ;
#1268 = CARTESIAN_POINT ( 'NONE',  ( 190.0000000000000853, 16.03993994372673626, 52.49999999999997868 ) ) ;
#1269 = VERTEX_POINT ( 'NONE', #11422 ) ;
#1270 = ORIENTED_EDGE ( 'NONE', *, *, #2769, .F. ) ;
#1271 = CARTESIAN_POINT ( 'NONE',  ( 190.0000000000000568, 15.03993994372673981, -2.575184203610571654 ) ) ;
#1272 = AXIS2_PLACEMENT_3D ( 'NONE', #6151, #7263, #117 ) ;
#1273 = ADVANCED_FACE ( 'NONE', ( #10242 ), #3060, .F. ) ;
#1274 = EDGE_LOOP ( 'NONE', ( #3424, #1499, #2007, #2831 ) ) ;
#1275 = CARTESIAN_POINT ( 'NONE',  ( 17.41029453487719181, 40.04259805664093363, 7.600000000000002309 ) ) ;
#1276 = AXIS2_PLACEMENT_3D ( 'NONE', #2453, #14444, #8319 ) ;
#1277 = CARTESIAN_POINT ( 'NONE',  ( -70.00000000000000000, 19.53993994372674337, -13.99999999999999289 ) ) ;
#1278 = ORIENTED_EDGE ( 'NONE', *, *, #6461, .T. ) ;
#1279 = ORIENTED_EDGE ( 'NONE', *, *, #10935, .F. ) ;
#1280 = CARTESIAN_POINT ( 'NONE',  ( -178.3861577417919477, 131.0834419243807076, -2.963320117457100888 ) ) ;
#1281 = EDGE_CURVE ( 'NONE', #11184, #10896, #473, .T. ) ;
#1282 = CARTESIAN_POINT ( 'NONE',  ( 201.1886137893777970, 49.58779752487713210, -5.375724496774349603 ) ) ;
#1283 = ORIENTED_EDGE ( 'NONE', *, *, #4940, .F. ) ;
#1284 = DIRECTION ( 'NONE',  ( -2.897122145519000304E-15, -0.9902680687415702510, -0.1391731009600660485 ) ) ;
#1285 = CYLINDRICAL_SURFACE ( 'NONE', #12239, 4.499999999999950262 ) ;
#1286 = CARTESIAN_POINT ( 'NONE',  ( 124.2806775638430281, 45.00321902537314145, 7.600000000000002309 ) ) ;
#1287 = AXIS2_PLACEMENT_3D ( 'NONE', #5372, #9089, #4100 ) ;
#1288 = STYLED_ITEM ( 'NONE', ( #11699 ), #563 ) ;
#1289 = ORIENTED_EDGE ( 'NONE', *, *, #2581, .F. ) ;
#1290 = EDGE_CURVE ( 'NONE', #2155, #10688, #5789, .T. ) ;
#1291 = CARTESIAN_POINT ( 'NONE',  ( 209.6520103264654438, 47.93571987055528183, -2.624305162434556582 ) ) ;
#1292 = ORIENTED_EDGE ( 'NONE', *, *, #10887, .T. ) ;
#1293 = DIRECTION ( 'NONE',  ( -1.000000000000000000, 0.000000000000000000, 0.000000000000000000 ) ) ;
#1294 = CARTESIAN_POINT ( 'NONE',  ( -81.74955057502458544, 65.19100426474074084, 10.00000000000000178 ) ) ;
#1295 = CARTESIAN_POINT ( 'NONE',  ( -200.9709139173866959, 128.5579952147370761, 5.434137442415933883 ) ) ;
#1296 = CARTESIAN_POINT ( 'NONE',  ( -157.6477983077465694, 110.1970436846185066, -5.000000000000000000 ) ) ;
#1297 = ORIENTED_EDGE ( 'NONE', *, *, #3867, .T. ) ;
#1298 = CARTESIAN_POINT ( 'NONE',  ( -216.9711578880983893, 150.1110767499728240, 9.578254705571840333 ) ) ;
#1300 = CARTESIAN_POINT ( 'NONE',  ( 114.0000000000000568, 64.53993994372673626, 11.47500000000035136 ) ) ;
#1299 = MECHANICAL_DESIGN_GEOMETRIC_PRESENTATION_REPRESENTATION (  '', ( #2837 ), #1309 ) ;
#1301 = ORIENTED_EDGE ( 'NONE', *, *, #4197, .T. ) ;
#1302 = ORIENTED_EDGE ( 'NONE', *, *, #9805, .T. ) ;
#1303 = AXIS2_PLACEMENT_3D ( 'NONE', #9004, #12617, #1876 ) ;
#1304 = DIRECTION ( 'NONE',  ( 0.000000000000000000, 1.000000000000000000, 0.000000000000000000 ) ) ;
#1305 = DIRECTION ( 'NONE',  ( 1.000000000000000000, 0.000000000000000000, 0.000000000000000000 ) ) ;
#1306 = CARTESIAN_POINT ( 'NONE',  ( 5.000000000000000000, 6.123233995736766282E-16, 5.000000000000000000 ) ) ;
#1307 = CARTESIAN_POINT ( 'NONE',  ( -110.0000000000000426, 59.53993994372674337, 10.00000000000000178 ) ) ;
#1308 = CARTESIAN_POINT ( 'NONE',  ( -225.6439726407676005, 142.9626156777225390, 1.090105839479173833 ) ) ;
#1309 =( GEOMETRIC_REPRESENTATION_CONTEXT ( 3 ) GLOBAL_UNCERTAINTY_ASSIGNED_CONTEXT ( ( #1691 ) ) GLOBAL_UNIT_ASSIGNED_CONTEXT ( ( #4692, #15567, #9444 ) ) REPRESENTATION_CONTEXT ( 'NONE', 'WORKASPACE' ) );
#1310 = EDGE_CURVE ( 'NONE', #2929, #12060, #10398, .T. ) ;
#1311 = EDGE_CURVE ( 'NONE', #1809, #4918, #8825, .T. ) ;
#1312 = FACE_OUTER_BOUND ( 'NONE', #2942, .T. ) ;
#1313 = EDGE_CURVE ( 'NONE', #9986, #11722, #5261, .T. ) ;
#1314 = AXIS2_PLACEMENT_3D ( 'NONE', #11044, #9473, #2518 ) ;
#1315 = CARTESIAN_POINT ( 'NONE',  ( -157.5246693090277006, 109.6988848934566647, 9.252772226370421293 ) ) ;
#1316 = CARTESIAN_POINT ( 'NONE',  ( -198.5677679834141713, 144.7676449960911498, 2.500000000000000000 ) ) ;
#1317 = DIRECTION ( 'NONE',  ( -0.000000000000000000, 1.000000000000000000, -0.000000000000000000 ) ) ;
#1318 = DIRECTION ( 'NONE',  ( 1.000000000000000000, 0.000000000000000000, 0.000000000000000000 ) ) ;
#1319 = EDGE_LOOP ( 'NONE', ( #14221, #12598, #7572, #3944 ) ) ;
#1320 = ORIENTED_EDGE ( 'NONE', *, *, #15180, .T. ) ;
#1321 = CYLINDRICAL_SURFACE ( 'NONE', #6253, 1.700000000000007061 ) ;
#1322 = CARTESIAN_POINT ( 'NONE',  ( 200.1062858801516597, 40.86394065090267702, 16.00000000000001421 ) ) ;
#1323 = CARTESIAN_POINT ( 'NONE',  ( -63.50000000000002842, 15.03993994372673981, 10.05257423913146475 ) ) ;
#1324 = CARTESIAN_POINT ( 'NONE',  ( -110.0000000000000426, 19.53993994372674337, 9.999999999999998224 ) ) ;
#1325 = FACE_BOUND ( 'NONE', #9221, .T. ) ;
#1326 = DIRECTION ( 'NONE',  ( 0.000000000000000000, 0.000000000000000000, 1.000000000000000000 ) ) ;
#1327 = CARTESIAN_POINT ( 'NONE',  ( 164.0000000000000568, 64.53993994372673626, 11.50000000000000000 ) ) ;
#1328 = VERTEX_POINT ( 'NONE', #15343 ) ;
#1329 = AXIS2_PLACEMENT_3D ( 'NONE', #12163, #3878, #2537 ) ;
#1330 = ORIENTED_EDGE ( 'NONE', *, *, #8852, .T. ) ;
#1331 = CARTESIAN_POINT ( 'NONE',  ( 208.8253499713366352, 39.76173270276598970, -9.127040822819912691 ) ) ;
#1332 = FACE_BOUND ( 'NONE', #3235, .T. ) ;
#1333 = VERTEX_POINT ( 'NONE', #7170 ) ;
#1334 = CIRCLE ( 'NONE', #10421, 0.5000000000000001110 ) ;
#1335 = CARTESIAN_POINT ( 'NONE',  ( -224.2877105866247973, 145.3925720454151929, 5.086385912607861215 ) ) ;
#1336 = ORIENTED_EDGE ( 'NONE', *, *, #8208, .T. ) ;
#1337 = DIRECTION ( 'NONE',  ( 0.000000000000000000, 0.000000000000000000, -1.000000000000000000 ) ) ;
#1338 = CARTESIAN_POINT ( 'NONE',  ( 14.00000000000004086, 62.13993994372673768, 13.30000000000105054 ) ) ;
#1340 = EDGE_LOOP ( 'NONE', ( #7669, #13345 ) ) ;
#1339 = VECTOR ( 'NONE', #10249, 1000.000000000000000 ) ;
#1341 = CARTESIAN_POINT ( 'NONE',  ( 70.26535645333922275, 38.79159067395544014, 10.00000000000000178 ) ) ;
#1342 = CARTESIAN_POINT ( 'NONE',  ( -220.3531759299249302, 148.3382346779569616, 2.431557144026069928 ) ) ;
#1343 = ADVANCED_FACE ( 'NONE', ( #11973 ), #5969, .F. ) ;
#1344 = ADVANCED_FACE ( 'NONE', ( #14014 ), #5891, .T. ) ;
#1345 = CARTESIAN_POINT ( 'NONE',  ( 0.000000000000000000, 0.000000000000000000, 0.000000000000000000 ) ) ;
#1346 = ORIENTED_EDGE ( 'NONE', *, *, #14428, .T. ) ;
#1347 = AXIS2_PLACEMENT_3D ( 'NONE', #14029, #8142, #8292 ) ;
#1348 = ORIENTED_EDGE ( 'NONE', *, *, #804, .T. ) ;
#1349 = DIRECTION ( 'NONE',  ( -0.000000000000000000, -0.000000000000000000, -1.000000000000000000 ) ) ;
#1350 = CARTESIAN_POINT ( 'NONE',  ( -64.00000000000002842, -178.8058001507315566, 52.19066787724494816 ) ) ;
#1351 = CARTESIAN_POINT ( 'NONE',  ( -157.0972765366304316, 120.0943610593438251, 0.000000000000000000 ) ) ;
#1352 = CARTESIAN_POINT ( 'NONE',  ( -150.8031737844540601, 108.0798160477858261, -4.962432776364140707 ) ) ;
#1353 = ORIENTED_EDGE ( 'NONE', *, *, #12446, .F. ) ;
#1354 = VERTEX_POINT ( 'NONE', #2100 ) ;
#1355 = CARTESIAN_POINT ( 'NONE',  ( -188.7806045336324132, 137.2844789098840863, -2.963320117457101777 ) ) ;
#1356 = CARTESIAN_POINT ( 'NONE',  ( 205.5168546899054434, 47.82311440310952833, -1.064259200291542529 ) ) ;
#1357 = AXIS2_PLACEMENT_3D ( 'NONE', #383, #763, #10414 ) ;
#1358 = VERTEX_POINT ( 'NONE', #7088 ) ;
#1359 = AXIS2_PLACEMENT_3D ( 'NONE', #7035, #4487, #13008 ) ;
#1360 = CARTESIAN_POINT ( 'NONE',  ( 178.0000000000000853, -179.3058001507315566, -51.45141194869120227 ) ) ;
#1361 = FACE_OUTER_BOUND ( 'NONE', #1656, .T. ) ;
#1362 = DIRECTION ( 'NONE',  ( 0.000000000000000000, 0.000000000000000000, -1.000000000000000000 ) ) ;
#1363 = ORIENTED_EDGE ( 'NONE', *, *, #5674, .T. ) ;
#1364 = ADVANCED_FACE ( 'NONE', ( #11665 ), #11815, .F. ) ;
#1365 = AXIS2_PLACEMENT_3D ( 'NONE', #660, #14086, #4220 ) ;
#1366 = CARTESIAN_POINT ( 'NONE',  ( 190.5757627275658876, 33.76246512414177658, -1.122914728280356433 ) ) ;
#1367 = ORIENTED_EDGE ( 'NONE', *, *, #6082, .F. ) ;
#1368 = CARTESIAN_POINT ( 'NONE',  ( -70.00000000000000000, 17.53993994372673271, 48.99999999999997158 ) ) ;
#1369 = CARTESIAN_POINT ( 'NONE',  ( -216.7159361415700403, 154.8568568287998630, 1.560284994380096046 ) ) ;
#1370 = CARTESIAN_POINT ( 'NONE',  ( -183.9200705329474772, 121.1751083001002485, -2.964974570226829087 ) ) ;
#1371 = CARTESIAN_POINT ( 'NONE',  ( 170.6931741512129577, -3.595212766542494887, -13.46247879130521952 ) ) ;
#1372 = ORIENTED_EDGE ( 'NONE', *, *, #9556, .F. ) ;
#1373 = CARTESIAN_POINT ( 'NONE',  ( -212.4168668197547731, 139.5435760318306677, 9.577123744044230946 ) ) ;
#1374 = CARTESIAN_POINT ( 'NONE',  ( 201.3430548014149792, 49.57506994421799362, -2.237714600605053228 ) ) ;
#1375 = EDGE_LOOP ( 'NONE', ( #15098, #949, #3175, #1346 ) ) ;
#1376 = ORIENTED_EDGE ( 'NONE', *, *, #7639, .F. ) ;
#1377 = CONICAL_SURFACE ( 'NONE', #8712, 3.525000000000002132, 0.7853981633974482790 ) ;
#1378 = EDGE_CURVE ( 'NONE', #4070, #14472, #12986, .T. ) ;
#1379 = CARTESIAN_POINT ( 'NONE',  ( 4.007948148170534052E-15, 0.3912769056150322000, 8.000000000000007105 ) ) ;
#1380 = DIRECTION ( 'NONE',  ( 1.000000000000000000, -2.751328491981765035E-32, 3.965082230804130220E-16 ) ) ;
#1381 = DIRECTION ( 'NONE',  ( -0.000000000000000000, -0.000000000000000000, 1.000000000000000000 ) ) ;
#1382 = DIRECTION ( 'NONE',  ( 0.000000000000000000, -0.000000000000000000, 1.000000000000000000 ) ) ;
#1383 = DIRECTION ( 'NONE',  ( 1.000000000000000000, 0.000000000000000000, 0.000000000000000000 ) ) ;
#1384 = AXIS2_PLACEMENT_3D ( 'NONE', #4184, #7925, #11302 ) ;
#1385 = CARTESIAN_POINT ( 'NONE',  ( -169.9361637590235716, 128.7768979049109532, 3.478855110294483133 ) ) ;
#1386 = CARTESIAN_POINT ( 'NONE',  ( 169.1145417280692698, 64.59938046134368506, -0.9107274384406877088 ) ) ;
#1387 = CARTESIAN_POINT ( 'NONE',  ( 0.000000000000000000, 0.000000000000000000, 0.000000000000000000 ) ) ;
#1388 = EDGE_LOOP ( 'NONE', ( #7148, #8695 ) ) ;
#1389 = AXIS2_PLACEMENT_3D ( 'NONE', #6841, #13934, #11495 ) ;
#1390 = EDGE_CURVE ( 'NONE', #14442, #4447, #3528, .T. ) ;
#1391 = EDGE_LOOP ( 'NONE', ( #428, #6702, #6658, #10982 ) ) ;
#1392 = LINE ( 'NONE', #3931, #8028 ) ;
#1393 = CARTESIAN_POINT ( 'NONE',  ( -31.29899788034579089, 48.72489408690345414, 7.600000000000002309 ) ) ;
#1394 = FACE_OUTER_BOUND ( 'NONE', #1997, .T. ) ;
#1395 = CARTESIAN_POINT ( 'NONE',  ( -35.99999999999995026, 64.53993994372673626, 11.47500000000139941 ) ) ;
#1396 = CARTESIAN_POINT ( 'NONE',  ( 70.26535645333922275, 38.79159067395544014, 5.000000000000000000 ) ) ;
#1398 = EDGE_CURVE ( 'NONE', #11305, #13329, #8573, .T. ) ;
#1397 = EDGE_CURVE ( 'NONE', #14981, #13397, #2338, .T. ) ;
#1399 = ADVANCED_FACE ( 'NONE', ( #14319 ), #2015, .F. ) ;
#1400 = DIRECTION ( 'NONE',  ( 1.000000000000000000, 0.000000000000000000, -0.000000000000000000 ) ) ;
#1401 = DIRECTION ( 'NONE',  ( -0.000000000000000000, 0.4999999999999991118, -0.8660254037844390407 ) ) ;
#1402 = AXIS2_PLACEMENT_3D ( 'NONE', #5598, #4400, #13879 ) ;
#1403 = EDGE_CURVE ( 'NONE', #5373, #11059, #4546, .T. ) ;
#1404 = ORIENTED_EDGE ( 'NONE', *, *, #8963, .T. ) ;
#1405 = CARTESIAN_POINT ( 'NONE',  ( 200.1062858801516597, 47.86394065090266992, 12.00000000000001066 ) ) ;
#1406 = CARTESIAN_POINT ( 'NONE',  ( 194.7298858349713271, 47.80990288192585780, -8.002378029496236778 ) ) ;
#1407 = CARTESIAN_POINT ( 'NONE',  ( -221.6235305807591658, 150.1658687316387670, 7.893372954062758851 ) ) ;
#1408 = ORIENTED_EDGE ( 'NONE', *, *, #10370, .F. ) ;
#1409 = CARTESIAN_POINT ( 'NONE',  ( -224.3998921539632931, 145.1915811579927151, 4.610672262717653069 ) ) ;
#1410 = ORIENTED_EDGE ( 'NONE', *, *, #1015, .T. ) ;
#1411 = CARTESIAN_POINT ( 'NONE',  ( -171.8695707977107645, 120.3013568790891554, -4.955367435459418601 ) ) ;
#1412 = CIRCLE ( 'NONE', #10253, 0.5000000000000000000 ) ;
#1413 = CARTESIAN_POINT ( 'NONE',  ( 209.5813200025016840, 33.68906342850529256, -7.816773541869418196 ) ) ;
#1414 = AXIS2_PLACEMENT_3D ( 'NONE', #7818, #12607, #6634 ) ;
#1415 = EDGE_CURVE ( 'NONE', #11153, #5773, #6043, .T. ) ;
#1416 = ORIENTED_EDGE ( 'NONE', *, *, #11845, .F. ) ;
#1417 = ADVANCED_FACE ( 'NONE', ( #13136 ), #14354, .T. ) ;
#1418 = DIRECTION ( 'NONE',  ( -1.000000000000000000, -0.000000000000000000, -0.000000000000000000 ) ) ;
#1419 = CARTESIAN_POINT ( 'NONE',  ( -76.00000000000004263, 16.03993994372673626, 52.49999999999997868 ) ) ;
#1420 = CARTESIAN_POINT ( 'NONE',  ( -34.79899788034579444, 48.72489408690345414, 10.00000000000000178 ) ) ;
#1421 = ORIENTED_EDGE ( 'NONE', *, *, #1403, .T. ) ;
#1422 = EDGE_CURVE ( 'NONE', #207, #11026, #1141, .T. ) ;
#1423 =( NAMED_UNIT ( * ) SI_UNIT ( $, .STERADIAN. ) SOLID_ANGLE_UNIT ( ) );
#1424 = ORIENTED_EDGE ( 'NONE', *, *, #9453, .T. ) ;
#1425 = CYLINDRICAL_SURFACE ( 'NONE', #3896, 3.500000000000004885 ) ;
#1426 = VERTEX_POINT ( 'NONE', #8206 ) ;
#1427 = DIRECTION ( 'NONE',  ( 0.000000000000000000, 0.000000000000000000, -1.000000000000000000 ) ) ;
#1428 = ADVANCED_FACE ( 'NONE', ( #5661 ), #8831, .F. ) ;
#1429 = DIRECTION ( 'NONE',  ( -0.000000000000000000, 1.000000000000000000, 1.156482317317871725E-16 ) ) ;
#1430 = ORIENTED_EDGE ( 'NONE', *, *, #13657, .T. ) ;
#1431 = ORIENTED_EDGE ( 'NONE', *, *, #9842, .T. ) ;
#1432 = CARTESIAN_POINT ( 'NONE',  ( -195.9617019660094570, 137.8802668252396586, -4.640918829492428621 ) ) ;
#1433 = CARTESIAN_POINT ( 'NONE',  ( 193.1265229109121435, 35.50728864820005981, -5.680987958736793075 ) ) ;
#1434 = VERTEX_POINT ( 'NONE', #11741 ) ;
#1435 = CARTESIAN_POINT ( 'NONE',  ( -155.6745145678418680, 109.9335888524736049, -4.794633519332698768 ) ) ;
#1436 = LINE ( 'NONE', #14853, #10494 ) ;
#1437 = FACE_OUTER_BOUND ( 'NONE', #8455, .T. ) ;
#1438 = AXIS2_PLACEMENT_3D ( 'NONE', #15216, #5529, #12694 ) ;
#1439 = CARTESIAN_POINT ( 'NONE',  ( 191.3907470605235801, 42.09736693221333326, -1.487451979171016125 ) ) ;
#1440 = ORIENTED_EDGE ( 'NONE', *, *, #5443, .T. ) ;
#1441 = CARTESIAN_POINT ( 'NONE',  ( 190.5000000000000853, 15.53993994372673626, 52.49999999999997868 ) ) ;
#1442 = CARTESIAN_POINT ( 'NONE',  ( -217.5100339609262221, 153.4805093641580527, -2.286312808770087912 ) ) ;
#1443 = CIRCLE ( 'NONE', #3225, 1.699999999999991518 ) ;
#1444 = CARTESIAN_POINT ( 'NONE',  ( -205.6342130761154863, 139.8173426991758959, -5.230826428279590878 ) ) ;
#1445 = EDGE_CURVE ( 'NONE', #4264, #5504, #10547, .T. ) ;
#1446 = DIRECTION ( 'NONE',  ( 1.000000000000000000, 0.000000000000000000, 0.000000000000000000 ) ) ;
#1447 = VERTEX_POINT ( 'NONE', #2261 ) ;
#1448 = CARTESIAN_POINT ( 'NONE',  ( -181.1823003367078115, 126.0769834546670296, 10.16010209732750624 ) ) ;
#1449 = CARTESIAN_POINT ( 'NONE',  ( 205.4081958545874613, 47.87064854543508829, -4.057643371672452481 ) ) ;
#1450 = ORIENTED_EDGE ( 'NONE', *, *, #14813, .F. ) ;
#1451 = ORIENTED_EDGE ( 'NONE', *, *, #9650, .T. ) ;
#1452 = CIRCLE ( 'NONE', #14308, 4.172000000000013920 ) ;
#1453 = CARTESIAN_POINT ( 'NONE',  ( 0.000000000000000000, 0.000000000000000000, 5.000000000000000000 ) ) ;
#1454 = DIRECTION ( 'NONE',  ( 0.000000000000000000, 0.000000000000000000, 1.000000000000000000 ) ) ;
#1455 = DIRECTION ( 'NONE',  ( -1.000000000000000000, 0.000000000000000000, 0.000000000000000000 ) ) ;
#1456 = VECTOR ( 'NONE', #9861, 1000.000000000000000 ) ;
#1457 = CARTESIAN_POINT ( 'NONE',  ( 184.0000000000000568, 17.53993994372673271, 47.49999999999997868 ) ) ;
#1458 = DIRECTION ( 'NONE',  ( 0.000000000000000000, 0.000000000000000000, 1.000000000000000000 ) ) ;
#1459 = VECTOR ( 'NONE', #9027, 1000.000000000000000 ) ;
#1460 = CARTESIAN_POINT ( 'NONE',  ( -186.0759242617834559, 135.7072545306847076, 7.919662025281895446 ) ) ;
#1461 = CARTESIAN_POINT ( 'NONE',  ( -85.99999999999994316, 64.53993994372673626, 15.00000000000174794 ) ) ;
#1462 = CARTESIAN_POINT ( 'NONE',  ( 0.000000000000000000, 0.000000000000000000, 0.000000000000000000 ) ) ;
#1463 = ORIENTED_EDGE ( 'NONE', *, *, #6997, .F. ) ;
#1464 = ADVANCED_FACE ( 'NONE', ( #10714 ), #13058, .T. ) ;
#1465 = PLANE ( 'NONE',  #11873 ) ;
#1466 = VECTOR ( 'NONE', #14942, 1000.000000000000000 ) ;
#1467 = VERTEX_POINT ( 'NONE', #8361 ) ;
#1468 = B_SPLINE_CURVE_WITH_KNOTS ( 'NONE', 3,
 ( #4611, #14305, #969, #1131, #5799, #10777 ),
 .UNSPECIFIED., .F., .F.,
 ( 4, 2, 4 ),
 ( 2.380731630171312408E-07, 0.002336973833157586326, 0.004673709593152155714 ),
 .UNSPECIFIED. ) ;
#1469 = VERTEX_POINT ( 'NONE', #3451 ) ;
#1470 = CARTESIAN_POINT ( 'NONE',  ( 14.00000000000004086, 56.53993994372675047, 15.00000000000104983 ) ) ;
#1471 = CARTESIAN_POINT ( 'NONE',  ( 184.0000000000000568, 17.53993994372673981, -12.49999999999999289 ) ) ;
#1472 = CARTESIAN_POINT ( 'NONE',  ( 122.5806775638430253, 45.00321902537314145, 10.00000000000000178 ) ) ;
#1473 = DIRECTION ( 'NONE',  ( 0.000000000000000000, -0.000000000000000000, -1.000000000000000000 ) ) ;
#1474 = DIRECTION ( 'NONE',  ( 0.000000000000000000, 0.000000000000000000, 1.000000000000000000 ) ) ;
#1475 = DIRECTION ( 'NONE',  ( 0.000000000000000000, 0.000000000000000000, -1.000000000000000000 ) ) ;
#1476 = CARTESIAN_POINT ( 'NONE',  ( -86.97455057502459397, 65.19100426474074084, 10.00000000000000178 ) ) ;
#1477 = CARTESIAN_POINT ( 'NONE',  ( -206.2408270422487249, 148.5277750773568926, 5.434754235172608361 ) ) ;
#1478 = AXIS2_PLACEMENT_3D ( 'NONE', #14443, #7364, #12159 ) ;
#1480 = ORIENTED_EDGE ( 'NONE', *, *, #734, .F. ) ;
#1479 = EDGE_CURVE ( 'NONE', #9446, #12308, #13088, .T. ) ;
#1481 = AXIS2_PLACEMENT_3D ( 'NONE', #13040, #2164, #11802 ) ;
#1482 = VECTOR ( 'NONE', #15073, 1000.000000000000000 ) ;
#1483 = DIRECTION ( 'NONE',  ( 1.000000000000000000, 0.000000000000000000, 0.000000000000000000 ) ) ;
#1484 = EDGE_CURVE ( 'NONE', #5113, #9730, #1239, .T. ) ;
#1485 = CARTESIAN_POINT ( 'NONE',  ( 191.3918663844754349, 39.68659111044760124, -5.934329888686073140 ) ) ;
#1486 = PLANE ( 'NONE',  #8630 ) ;
#1487 = ORIENTED_EDGE ( 'NONE', *, *, #13530, .T. ) ;
#1488 = CIRCLE ( 'NONE', #11593, 0.4999999999999996114 ) ;
#1489 = EDGE_CURVE ( 'NONE', #13203, #2702, #11899, .T. ) ;
#1490 = CARTESIAN_POINT ( 'NONE',  ( -219.4551987602064855, 154.0507755588392911, 3.411546396426036409 ) ) ;
#1491 = ORIENTED_EDGE ( 'NONE', *, *, #8346, .T. ) ;
#1492 = CARTESIAN_POINT ( 'NONE',  ( -172.7841977562675311, 118.6626591106209787, -4.047107877712195823 ) ) ;
#1493 = CARTESIAN_POINT ( 'NONE',  ( 190.6654829352982290, 48.12161981134465805, -3.320406740534335377 ) ) ;
#1494 = ORIENTED_EDGE ( 'NONE', *, *, #10730, .T. ) ;
#1495 = CARTESIAN_POINT ( 'NONE',  ( 64.00000000000005684, 62.13993994372673768, 18.50000000000070344 ) ) ;
#1496 = CARTESIAN_POINT ( 'NONE',  ( 114.0000000000000568, 62.13993994372673768, 18.50000000000035527 ) ) ;
#1497 = CIRCLE ( 'NONE', #10338, 9.999999999999994671 ) ;
#1498 = FACE_OUTER_BOUND ( 'NONE', #14969, .T. ) ;
#1499 = ORIENTED_EDGE ( 'NONE', *, *, #9175, .T. ) ;
#1500 = VECTOR ( 'NONE', #644, 1000.000000000000000 ) ;
#1501 = AXIS2_PLACEMENT_3D ( 'NONE', #3784, #2757, #6235 ) ;
#1502 = CARTESIAN_POINT ( 'NONE',  ( -70.00000000000000000, -177.3058001507315566, -41.45141194869120227 ) ) ;
#1503 = TOROIDAL_SURFACE ( 'NONE', #5559, 1.000000000000000000, 0.5000000000000000000 ) ;
#1504 = ORIENTED_EDGE ( 'NONE', *, *, #3354, .F. ) ;
#1505 = EDGE_CURVE ( 'NONE', #15035, #2448, #4359, .T. ) ;
#1506 = ADVANCED_FACE ( 'NONE', ( #11979 ), #5977, .F. ) ;
#1507 = LINE ( 'NONE', #10999, #2120 ) ;
#1508 = EDGE_CURVE ( 'NONE', #11510, #12123, #1497, .T. ) ;
#1509 = CARTESIAN_POINT ( 'NONE',  ( -156.1541198758405358, 111.0769426152140369, 9.827040175762295604 ) ) ;
#1510 = EDGE_LOOP ( 'NONE', ( #2556, #9343, #9484, #11418, #10154 ) ) ;
#1511 = LINE ( 'NONE', #11231, #6713 ) ;
#1512 = DIRECTION ( 'NONE',  ( 0.000000000000000000, 0.000000000000000000, -1.000000000000000000 ) ) ;
#1513 = CIRCLE ( 'NONE', #7334, 0.5000000000000001110 ) ;
#1514 = ORIENTED_EDGE ( 'NONE', *, *, #14251, .T. ) ;
#1515 = ORIENTED_EDGE ( 'NONE', *, *, #10550, .F. ) ;
#1516 = LINE ( 'NONE', #14770, #5762 ) ;
#1517 = CARTESIAN_POINT ( 'NONE',  ( 207.1288103955774318, 46.12660085639766550, -4.186765234109192768 ) ) ;
#1518 = AXIS2_PLACEMENT_3D ( 'NONE', #7907, #11599, #764 ) ;
#1519 = EDGE_LOOP ( 'NONE', ( #9319, #15000, #14239, #408, #11238, #5624 ) ) ;
#1520 = DIRECTION ( 'NONE',  ( 0.000000000000000000, -3.469446951953611033E-15, 1.000000000000000000 ) ) ;
#1521 = CARTESIAN_POINT ( 'NONE',  ( 14.00000000000004086, 64.53993994372673626, 15.00000000000104983 ) ) ;
#1522 = DIRECTION ( 'NONE',  ( 0.000000000000000000, 0.000000000000000000, 1.000000000000000000 ) ) ;
#1523 = ADVANCED_FACE ( 'NONE', ( #15584 ), #7177, .F. ) ;
#1524 = CIRCLE ( 'NONE', #7851, 3.500000000000004885 ) ;
#1525 = AXIS2_PLACEMENT_3D ( 'NONE', #12830, #11509, #665 ) ;
#1526 = FACE_BOUND ( 'NONE', #14844, .T. ) ;
#1527 = CARTESIAN_POINT ( 'NONE',  ( 188.2965488188713721, 39.35787245461563089, -4.374714073396582137 ) ) ;
#1528 = ORIENTED_EDGE ( 'NONE', *, *, #856, .T. ) ;
#1529 = FACE_OUTER_BOUND ( 'NONE', #13428, .T. ) ;
#1530 = CARTESIAN_POINT ( 'NONE',  ( -220.2566479300740241, 148.4875731452288221, -5.069746451151177169 ) ) ;
#1531 = CARTESIAN_POINT ( 'NONE',  ( -212.3935931674892856, 139.5852744332111683, -4.642206099735020963 ) ) ;
#1532 = CARTESIAN_POINT ( 'NONE',  ( 6.399999999999999467, 4.618802153516981868, -7.999999999999979572 ) ) ;
#1533 = EDGE_LOOP ( 'NONE', ( #9557, #1537, #3772, #14772 ) ) ;
#1534 = CARTESIAN_POINT ( 'NONE',  ( -217.9748787080196450, 139.5740753954225966, -0.4555467707853197989 ) ) ;
#1535 = CARTESIAN_POINT ( 'NONE',  ( 198.9622538275367845, 49.57425033952682014, -2.112703922695001513 ) ) ;
#1536 = ORIENTED_EDGE ( 'NONE', *, *, #12679, .F. ) ;
#1537 = ORIENTED_EDGE ( 'NONE', *, *, #12204, .F. ) ;
#1538 = AXIS2_PLACEMENT_3D ( 'NONE', #14552, #13293, #7325 ) ;
#1539 = DIRECTION ( 'NONE',  ( 0.000000000000000000, 0.1391731009600584990, -0.9902680687415712502 ) ) ;
#1540 = LINE ( 'NONE', #2735, #7744 ) ;
#1541 = ADVANCED_FACE ( 'NONE', ( #1150, #3524, #988, #13143, #2345, #5740, #10554 ), #10797, .T. ) ;
#1542 = EDGE_CURVE ( 'NONE', #10751, #7203, #3606, .T. ) ;
#1543 = AXIS2_PLACEMENT_3D ( 'NONE', #2647, #7468, #13284 ) ;
#1544 = FACE_OUTER_BOUND ( 'NONE', #11818, .T. ) ;
#1545 = EDGE_CURVE ( 'NONE', #10399, #9297, #13597, .T. ) ;
#1546 = LINE ( 'NONE', #6381, #5145 ) ;
#1547 = TOROIDAL_SURFACE ( 'NONE', #5330, 1.000000000000000000, 0.5000000000000000000 ) ;
#1548 = DIRECTION ( 'NONE',  ( 1.000000000000000000, 0.000000000000000000, 0.000000000000000000 ) ) ;
#1549 = CARTESIAN_POINT ( 'NONE',  ( -218.4488137430494419, 155.8538722928748541, 3.478855109783925315 ) ) ;
#1550 = LINE ( 'NONE', #3854, #9543 ) ;
#1551 = AXIS2_PLACEMENT_3D ( 'NONE', #15520, #15282, #4640 ) ;
#1552 = LINE ( 'NONE', #13232, #4560 ) ;
#1553 = ORIENTED_EDGE ( 'NONE', *, *, #12044, .T. ) ;
#1554 = LINE ( 'NONE', #1787, #12369 ) ;
#1555 = ORIENTED_EDGE ( 'NONE', *, *, #1929, .F. ) ;
#1556 = ORIENTED_EDGE ( 'NONE', *, *, #3132, .T. ) ;
#1557 = CARTESIAN_POINT ( 'NONE',  ( -151.9345376450077367, 108.1333972819248004, 9.722517344254141491 ) ) ;
#1558 = DIRECTION ( 'NONE',  ( 0.000000000000000000, 0.000000000000000000, -1.000000000000000000 ) ) ;
#1559 = DIRECTION ( 'NONE',  ( 0.000000000000000000, -0.5000000000000019984, -0.8660254037844375974 ) ) ;
#1560 = LINE ( 'NONE', #8837, #1095 ) ;
#1561 = CARTESIAN_POINT ( 'NONE',  ( 190.5000000000000568, 16.03993994372673981, -17.50000000000002487 ) ) ;
#1562 = CIRCLE ( 'NONE', #9643, 0.5000000000000004441 ) ;
#1563 = DIRECTION ( 'NONE',  ( -0.000000000000000000, -0.000000000000000000, 1.000000000000000000 ) ) ;
#1564 = CARTESIAN_POINT ( 'NONE',  ( -185.3757041553864156, 136.9956776582455973, 5.434754235172603920 ) ) ;
#1565 = VERTEX_POINT ( 'NONE', #12048 ) ;
#1566 = PRODUCT_DEFINITION_CONTEXT ( 'detailed design', #10793, 'design' ) ;
#1567 = EDGE_CURVE ( 'NONE', #6280, #14008, #35, .T. ) ;
#1568 = DIRECTION ( 'NONE',  ( 0.000000000000000000, -1.000000000000000000, 0.000000000000000000 ) ) ;
#1569 = DIRECTION ( 'NONE',  ( 0.000000000000000000, 0.000000000000000000, -1.000000000000000000 ) ) ;
#1570 = ORIENTED_EDGE ( 'NONE', *, *, #1313, .F. ) ;
#1571 = CARTESIAN_POINT ( 'NONE',  ( -221.8318359980363539, 149.7926568781921048, 9.921711862944807336 ) ) ;
#1572 = VERTEX_POINT ( 'NONE', #8212 ) ;
#1573 = CARTESIAN_POINT ( 'NONE',  ( -108.0000000000000568, 59.53993994372674337, 10.00000000000000178 ) ) ;
#1574 = VECTOR ( 'NONE', #11068, 1000.000000000000000 ) ;
#1575 = DIRECTION ( 'NONE',  ( 1.000000000000000000, 0.000000000000000000, 0.000000000000000000 ) ) ;
#1576 = ORIENTED_EDGE ( 'NONE', *, *, #11922, .F. ) ;
#1577 = DIRECTION ( 'NONE',  ( 0.000000000000000000, -6.938893903907227145E-17, 1.000000000000000000 ) ) ;
#1578 = CYLINDRICAL_SURFACE ( 'NONE', #3049, 1.499999999999997780 ) ;
#1579 = ADVANCED_FACE ( 'NONE', ( #10057, #2953 ), #12645, .F. ) ;
#1580 = CARTESIAN_POINT ( 'NONE',  ( 14.00000000000004086, 59.53993994372674337, 15.00000000000104983 ) ) ;
#1581 = ORIENTED_EDGE ( 'NONE', *, *, #8363, .T. ) ;
#1582 = APPLICATION_PROTOCOL_DEFINITION ( 'draft international standard', 'automotive_design', 1998, #9991 ) ;
#1583 = CIRCLE ( 'NONE', #7152, 0.5000000000000001110 ) ;
#1584 = VERTEX_POINT ( 'NONE', #7772 ) ;
#1585 = AXIS2_PLACEMENT_3D ( 'NONE', #4159, #11516, #10332 ) ;
#1586 = DIRECTION ( 'NONE',  ( 0.000000000000000000, 0.000000000000000000, 1.000000000000000000 ) ) ;
#1587 = DIRECTION ( 'NONE',  ( -1.000000000000000000, 0.000000000000000000, 0.000000000000000000 ) ) ;
#1588 = ORIENTED_EDGE ( 'NONE', *, *, #4992, .F. ) ;
#1589 = CARTESIAN_POINT ( 'NONE',  ( -143.5695094297736034, 95.08739346018396077, 5.000000000000000000 ) ) ;
#1590 = CIRCLE ( 'NONE', #10426, 0.5000000000000004441 ) ;
#1591 = PLANE ( 'NONE',  #202 ) ;
#1592 = VERTEX_POINT ( 'NONE', #8588 ) ;
#1593 = ORIENTED_EDGE ( 'NONE', *, *, #7358, .F. ) ;
#1594 = CARTESIAN_POINT ( 'NONE',  ( -169.9274309510963406, 128.7925441011331031, 1.515441478317341994 ) ) ;
#1595 = CARTESIAN_POINT ( 'NONE',  ( 191.3844089520862894, 42.02011290432638901, -3.056456915890917170 ) ) ;
#1596 = ORIENTED_EDGE ( 'NONE', *, *, #13880, .T. ) ;
#1597 = CARTESIAN_POINT ( 'NONE',  ( 178.0000000000000853, 15.03993994372673981, -2.575184203610571654 ) ) ;
#1598 = DIRECTION ( 'NONE',  ( 0.9951762285753402715, -0.09810338464376282264, 0.000000000000000000 ) ) ;
#1599 = AXIS2_PLACEMENT_3D ( 'NONE', #10491, #6867, #11596 ) ;
#1600 = DIRECTION ( 'NONE',  ( -0.000000000000000000, -0.000000000000000000, -1.000000000000000000 ) ) ;
#1601 = LINE ( 'NONE', #4047, #634 ) ;
#1602 = EDGE_CURVE ( 'NONE', #15306, #9812, #3267, .T. ) ;
#1604 = EDGE_CURVE ( 'NONE', #956, #13999, #11477, .T. ) ;
#1603 = EDGE_CURVE ( 'NONE', #11059, #9376, #6576, .T. ) ;
#1605 = CARTESIAN_POINT ( 'NONE',  ( 190.0000000000000853, -179.8058001507315566, 84.88378295107887084 ) ) ;
#1606 = AXIS2_PLACEMENT_3D ( 'NONE', #5249, #1539, #1695 ) ;
#1607 = APPLICATION_CONTEXT ( 'automotive_design' ) ;
#1608 = EDGE_CURVE ( 'NONE', #6618, #13250, #10348, .T. ) ;
#1609 = DIRECTION ( 'NONE',  ( -0.4873681696970814659, -0.8731965799097686221, 0.000000000000000000 ) ) ;
#1610 = VERTEX_POINT ( 'NONE', #472 ) ;
#1611 = LINE ( 'NONE', #14705, #12641 ) ;
#1612 = CARTESIAN_POINT ( 'NONE',  ( -216.6980668629938123, 154.8869363267023687, 2.500000000158653091 ) ) ;
#1613 = AXIS2_PLACEMENT_3D ( 'NONE', #12528, #5520, #1722 ) ;
#1614 = CARTESIAN_POINT ( 'NONE',  ( -202.2493014528935475, 138.0335512477381883, -5.230826428279597096 ) ) ;
#1615 = DIRECTION ( 'NONE',  ( -1.000000000000000000, 0.000000000000000000, 0.000000000000000000 ) ) ;
#1616 = ORIENTED_EDGE ( 'NONE', *, *, #15191, .T. ) ;
#1617 = CARTESIAN_POINT ( 'NONE',  ( -194.2694872093395873, 127.5478817636406035, 5.434137442415935659 ) ) ;
#1618 = CARTESIAN_POINT ( 'NONE',  ( 191.3767946852191528, 39.76267059705192253, -4.365329018565075714 ) ) ;
#1619 =( GEOMETRIC_REPRESENTATION_CONTEXT ( 3 ) GLOBAL_UNCERTAINTY_ASSIGNED_CONTEXT ( ( #726 ) ) GLOBAL_UNIT_ASSIGNED_CONTEXT ( ( #3698, #15606, #6159 ) ) REPRESENTATION_CONTEXT ( 'NONE', 'WORKASPACE' ) );
#1620 = ORIENTED_EDGE ( 'NONE', *, *, #11583, .F. ) ;
#1621 = CARTESIAN_POINT ( 'NONE',  ( 0.3167204509598230411, -5.377136764700228611, -6.686525924292699763 ) ) ;
#1622 = DIRECTION ( 'NONE',  ( -0.000000000000000000, 1.000000000000000000, -0.000000000000000000 ) ) ;
#1623 = CARTESIAN_POINT ( 'NONE',  ( 2.000000000000000000, 3.175426480542944407, -3.252606517456511330E-16 ) ) ;
#1624 = AXIS2_PLACEMENT_3D ( 'NONE', #1082, #11907, #8594 ) ;
#1625 = EDGE_CURVE ( 'NONE', #11700, #462, #12561, .T. ) ;
#1626 = LINE ( 'NONE', #11114, #3622 ) ;
#1627 = ORIENTED_EDGE ( 'NONE', *, *, #9905, .T. ) ;
#1628 = CYLINDRICAL_SURFACE ( 'NONE', #6182, 1.700000000000007061 ) ;
#1629 = CARTESIAN_POINT ( 'NONE',  ( -169.2610106913410277, 124.9750017845142764, 2.431557144026069928 ) ) ;
#1630 = CARTESIAN_POINT ( 'NONE',  ( -156.8034031652508133, 111.1936819864191506, -4.924812526309167104 ) ) ;
#1631 = VERTEX_POINT ( 'NONE', #5314 ) ;
#1632 = DIRECTION ( 'NONE',  ( -1.000000000000000000, 0.000000000000000000, 0.000000000000000000 ) ) ;
#1633 = EDGE_CURVE ( 'NONE', #8949, #7872, #9856, .T. ) ;
#1634 = AXIS2_PLACEMENT_3D ( 'NONE', #15188, #12908, #6927 ) ;
#1635 = ORIENTED_EDGE ( 'NONE', *, *, #3279, .T. ) ;
#1636 = ORIENTED_EDGE ( 'NONE', *, *, #59, .T. ) ;
#1637 = CARTESIAN_POINT ( 'NONE',  ( -76.50000000000004263, 15.60952649420676686, 25.87720316414728217 ) ) ;
#1638 = DIRECTION ( 'NONE',  ( 1.000000000000000000, 0.000000000000000000, 0.000000000000000000 ) ) ;
#1639 = PLANE ( 'NONE',  #7391 ) ;
#1640 = DIRECTION ( 'NONE',  ( 0.000000000000000000, 0.000000000000000000, 1.000000000000000000 ) ) ;
#1641 = DIRECTION ( 'NONE',  ( -0.000000000000000000, 0.000000000000000000, 1.000000000000000000 ) ) ;
#1642 = DIRECTION ( 'NONE',  ( -0.000000000000000000, -4.956352788505162775E-17, 1.000000000000000000 ) ) ;
#1643 = CARTESIAN_POINT ( 'NONE',  ( -207.0940556909077657, 149.0079180481279479, 5.434754235172608361 ) ) ;
#1644 = EDGE_LOOP ( 'NONE', ( #4661, #10401 ) ) ;
#1645 = CYLINDRICAL_SURFACE ( 'NONE', #5383, 3.499999999999999556 ) ;
#1646 = DIRECTION ( 'NONE',  ( 1.000000000000000000, -4.585547486636276518E-32, 3.965082230804130220E-16 ) ) ;
#1647 = DIRECTION ( 'NONE',  ( -0.000000000000000000, 1.000000000000000000, -0.000000000000000000 ) ) ;
#1648 = ADVANCED_FACE ( 'NONE', ( #13749 ), #4122, .F. ) ;
#1649 = CARTESIAN_POINT ( 'NONE',  ( -224.5619881126438315, 144.9011608032434992, 1.476503984934130598 ) ) ;
#1650 = ORIENTED_EDGE ( 'NONE', *, *, #12484, .F. ) ;
#1651 = CARTESIAN_POINT ( 'NONE',  ( -220.7901307343587689, 151.6590353782033560, 9.451677507526856203 ) ) ;
#1652 = EDGE_LOOP ( 'NONE', ( #1257, #1825, #15285, #1440 ) ) ;
#1653 = CARTESIAN_POINT ( 'NONE',  ( -167.8131253141077650, 127.5691157174926644, 1.575245659892765326 ) ) ;
#1654 = LINE ( 'NONE', #15057, #16 ) ;
#1655 = AXIS2_PLACEMENT_3D ( 'NONE', #1589, #2630, #6426 ) ;
#1656 = EDGE_LOOP ( 'NONE', ( #3101, #4886, #14421, #13016 ) ) ;
#1657 = CARTESIAN_POINT ( 'NONE',  ( -76.00000000000004263, 15.03993994372673804, 38.07518420361041933 ) ) ;
#1658 = LINE ( 'NONE', #14827, #7342 ) ;
#1659 = VECTOR ( 'NONE', #10535, 1000.000000000000000 ) ;
#1660 = FACE_OUTER_BOUND ( 'NONE', #8338, .T. ) ;
#1661 = ORIENTED_EDGE ( 'NONE', *, *, #3705, .F. ) ;
#1662 = DIRECTION ( 'NONE',  ( 0.000000000000000000, 0.000000000000000000, 1.000000000000000000 ) ) ;
#1663 = ORIENTED_EDGE ( 'NONE', *, *, #1542, .T. ) ;
#1664 = CARTESIAN_POINT ( 'NONE',  ( 200.1062858801516597, 40.86394065090267702, 12.00000000000001066 ) ) ;
#1665 = CARTESIAN_POINT ( 'NONE',  ( -155.6477983077462568, 110.3268634018094758, 9.747367390575373491 ) ) ;
#1666 = EDGE_LOOP ( 'NONE', ( #7048, #3166, #11016, #2259, #104, #12408 ) ) ;
#1667 = TOROIDAL_SURFACE ( 'NONE', #3685, 1.000000000000000000, 0.5000000000000000000 ) ;
#1668 = CARTESIAN_POINT ( 'NONE',  ( -110.0000000000000426, 26.39124795404934076, 0.000000000000000000 ) ) ;
#1669 = AXIS2_PLACEMENT_3D ( 'NONE', #12201, #13386, #11188 ) ;
#1670 = EDGE_CURVE ( 'NONE', #9409, #14543, #3028, .T. ) ;
#1671 = DIRECTION ( 'NONE',  ( 3.965082230804130220E-16, 0.000000000000000000, 1.000000000000000000 ) ) ;
#1672 = EDGE_LOOP ( 'NONE', ( #11745, #12944 ) ) ;
#1673 = EDGE_LOOP ( 'NONE', ( #11669, #7615 ) ) ;
#1674 = CARTESIAN_POINT ( 'NONE',  ( 170.2911098586863545, 111.9959133412127272, 5.000000000000000000 ) ) ;
#1675 = CARTESIAN_POINT ( 'NONE',  ( 198.8863654052626657, 49.55881746625484396, -3.681704842056328086 ) ) ;
#1676 = ORIENTED_EDGE ( 'NONE', *, *, #12956, .T. ) ;
#1677 = DIRECTION ( 'NONE',  ( -3.965082230804130220E-16, 1.090924371466202084E-47, 1.000000000000000000 ) ) ;
#1678 = FACE_OUTER_BOUND ( 'NONE', #14769, .T. ) ;
#1679 = DIRECTION ( 'NONE',  ( -0.000000000000000000, 0.9902680687415705840, 0.1391731009600641333 ) ) ;
#1680 = CYLINDRICAL_SURFACE ( 'NONE', #15266, 1.500000000000001332 ) ;
#1681 = CARTESIAN_POINT ( 'NONE',  ( -34.79899788034579444, 48.72489408690345414, 10.00000000000000178 ) ) ;
#1682 = EDGE_CURVE ( 'NONE', #5329, #12823, #13351, .T. ) ;
#1683 = DIRECTION ( 'NONE',  ( -0.000000000000000000, 1.000000000000000000, -0.000000000000000000 ) ) ;
#1684 = ORIENTED_EDGE ( 'NONE', *, *, #278, .T. ) ;
#1685 = DIRECTION ( 'NONE',  ( -0.8204839007831801201, 0.5707893219124390294, -0.03171306586179811760 ) ) ;
#1686 = CARTESIAN_POINT ( 'NONE',  ( -223.4327756907198648, 142.3614043895485963, 0.01469651188060598634 ) ) ;
#1687 = CARTESIAN_POINT ( 'NONE',  ( -182.6467173238959560, 123.4549944991208292, -4.642206099735001423 ) ) ;
#1688 = CARTESIAN_POINT ( 'NONE',  ( 5.799999999999999822, 4.618802153516981868, 8.000000000000007105 ) ) ;
#1689 = ORIENTED_EDGE ( 'NONE', *, *, #1311, .T. ) ;
#1690 = CARTESIAN_POINT ( 'NONE',  ( -194.4337897068680547, 127.2572260587109554, 3.478895870929501033 ) ) ;
#1691 = UNCERTAINTY_MEASURE_WITH_UNIT (LENGTH_MEASURE( 1.000000000000000082E-05 ), #4692, 'distance_accuracy_value', 'NONE');
#1692 = CARTESIAN_POINT ( 'NONE',  ( 194.7047954745769687, 33.92018974228710704, -0.9908858387024377379 ) ) ;
#1693 = ORIENTED_EDGE ( 'NONE', *, *, #657, .F. ) ;
#1694 = ADVANCED_FACE ( 'NONE', ( #1678 ), #5396, .T. ) ;
#1695 = DIRECTION ( 'NONE',  ( 0.000000000000000000, 0.9902680687415712502, 0.1391731009600584990 ) ) ;
#1696 = DIRECTION ( 'NONE',  ( 0.000000000000000000, 4.956352788505162775E-17, -1.000000000000000000 ) ) ;
#1697 = DIRECTION ( 'NONE',  ( -0.000000000000000000, -0.000000000000000000, 1.000000000000000000 ) ) ;
#1698 = CIRCLE ( 'NONE', #3471, 3.499999999999999556 ) ;
#1699 = FACE_OUTER_BOUND ( 'NONE', #1894, .T. ) ;
#1700 = VERTEX_POINT ( 'NONE', #14929 ) ;
#1701 = CARTESIAN_POINT ( 'NONE',  ( -31.29899788034579089, 48.72489408690345414, 10.00000000000000178 ) ) ;
#1702 = EDGE_CURVE ( 'NONE', #14752, #11943, #3760, .T. ) ;
#1703 = ADVANCED_FACE ( 'NONE', ( #7698 ), #12487, .F. ) ;
#1704 = CARTESIAN_POINT ( 'NONE',  ( -76.50000000000004263, 17.53993994372673626, 52.49999999999997868 ) ) ;
#1705 = DIRECTION ( 'NONE',  ( 0.000000000000000000, 0.000000000000000000, -1.000000000000000000 ) ) ;
#1706 = PRODUCT_DEFINITION_SHAPE ( 'NONE', 'NONE',  #4976 ) ;
#1707 = ORIENTED_EDGE ( 'NONE', *, *, #4864, .T. ) ;
#1708 = CARTESIAN_POINT ( 'NONE',  ( -5.196152422706630247, -9.000000000000005329, 5.000000000000000000 ) ) ;
#1709 = ORIENTED_EDGE ( 'NONE', *, *, #11072, .F. ) ;
#1710 = EDGE_LOOP ( 'NONE', ( #1528, #10910, #10729, #12950 ) ) ;
#1711 = DIRECTION ( 'NONE',  ( -3.965082230804130220E-16, -4.956352788505162775E-17, 1.000000000000000000 ) ) ;
#1712 = DIRECTION ( 'NONE',  ( 1.000000000000000000, 0.000000000000000000, 0.000000000000000000 ) ) ;
#1713 = AXIS2_PLACEMENT_3D ( 'NONE', #5111, #12137, #8746 ) ;
#1714 = DIRECTION ( 'NONE',  ( -0.000000000000000000, 1.000000000000000000, -0.000000000000000000 ) ) ;
#1715 = DIRECTION ( 'NONE',  ( 0.000000000000000000, 4.956352788505162775E-17, -1.000000000000000000 ) ) ;
#1716 = CARTESIAN_POINT ( 'NONE',  ( -219.5038107907490144, 153.9636794753398874, -2.869066018171615884 ) ) ;
#1717 = FACE_OUTER_BOUND ( 'NONE', #9914, .T. ) ;
#1718 = ORIENTED_EDGE ( 'NONE', *, *, #4489, .F. ) ;
#1719 = EDGE_CURVE ( 'NONE', #3938, #7406, #5234, .T. ) ;
#1720 = TOROIDAL_SURFACE ( 'NONE', #10807, 1.000000000000000000, 0.5000000000000000000 ) ;
#1721 = PRODUCT_DEFINITION_FORMATION_WITH_SPECIFIED_SOURCE ( 'ANY', '', #8040, .NOT_KNOWN. ) ;
#1722 = DIRECTION ( 'NONE',  ( 1.000000000000000000, 0.000000000000000000, 0.000000000000000000 ) ) ;
#1723 = VECTOR ( 'NONE', #12040, 1000.000000000000000 ) ;
#1724 = DIRECTION ( 'NONE',  ( 1.000000000000000000, -2.751328491981765035E-32, 3.965082230804130220E-16 ) ) ;
#1725 = CARTESIAN_POINT ( 'NONE',  ( -223.5023877966752366, 146.7996010984935538, -2.058674290867560153 ) ) ;
#1726 = EDGE_LOOP ( 'NONE', ( #15460, #12803, #6817, #4219 ) ) ;
#1727 = CARTESIAN_POINT ( 'NONE',  ( -219.7785425680613400, 153.4714543706508891, 5.235913750827374535 ) ) ;
#1728 = ORIENTED_EDGE ( 'NONE', *, *, #5273, .F. ) ;
#1729 = CARTESIAN_POINT ( 'NONE',  ( -168.3225553318488892, 126.6563918736861325, -1.708925576422542392 ) ) ;
#1730 = CARTESIAN_POINT ( 'NONE',  ( 190.0000000000000568, -178.8058001507315566, 52.19066787724494816 ) ) ;
#1731 = VERTEX_POINT ( 'NONE', #11313 ) ;
#1732 = DIRECTION ( 'NONE',  ( 0.000000000000000000, 0.000000000000000000, -1.000000000000000000 ) ) ;
#1733 = CARTESIAN_POINT ( 'NONE',  ( -1.820951430007294553E-14, 7.321656987762852786, -3.318518101602990988 ) ) ;
#1734 = CIRCLE ( 'NONE', #10562, 6.999999999999978684 ) ;
#1735 = CIRCLE ( 'NONE', #12316, 5.000000000000000000 ) ;
#1736 = EDGE_CURVE ( 'NONE', #10382, #2412, #10093, .T. ) ;
#1737 = LINE ( 'NONE', #10040, #3352 ) ;
#1738 = EDGE_LOOP ( 'NONE', ( #1372, #10188, #13821, #11406 ) ) ;
#1739 = APPLICATION_PROTOCOL_DEFINITION ( 'draft international standard', 'automotive_design', 1998, #11595 ) ;
#1740 = ORIENTED_EDGE ( 'NONE', *, *, #9984, .T. ) ;
#1741 = VECTOR ( 'NONE', #7234, 1000.000000000000000 ) ;
#1742 = CARTESIAN_POINT ( 'NONE',  ( 205.1062858801516597, 40.86394065090267702, 0.000000000000000000 ) ) ;
#1743 = EDGE_LOOP ( 'NONE', ( #13760, #10131, #807, #7421 ) ) ;
#1744 = CARTESIAN_POINT ( 'NONE',  ( -144.0627431139473345, 95.36268816863731956, 5.000000000000000000 ) ) ;
#1745 = AXIS2_PLACEMENT_3D ( 'NONE', #5566, #11325, #7871 ) ;
#1746 = DIRECTION ( 'NONE',  ( 1.000000000000000000, -2.751328491981765035E-32, 3.965082230804130220E-16 ) ) ;
#1747 = ORIENTED_EDGE ( 'NONE', *, *, #9225, .F. ) ;
#1748 = ORIENTED_EDGE ( 'NONE', *, *, #6543, .F. ) ;
#1749 = CARTESIAN_POINT ( 'NONE',  ( 177.5000000000000853, 17.53993994372673626, 52.49999999999997868 ) ) ;
#1750 = CARTESIAN_POINT ( 'NONE',  ( -35.99999999999995026, 56.53993994372675047, 15.00000000000139977 ) ) ;
#1751 = ORIENTED_EDGE ( 'NONE', *, *, #2238, .F. ) ;
#1753 = EDGE_CURVE ( 'NONE', #1584, #14280, #107, .T. ) ;
#1752 = CARTESIAN_POINT ( 'NONE',  ( 193.1249951165660548, 46.22013307728793308, -3.310989833511668756 ) ) ;
#1754 = DIRECTION ( 'NONE',  ( -0.2258817899775119320, -0.9741547192086866813, 0.000000000000000000 ) ) ;
#1755 = AXIS2_PLACEMENT_3D ( 'NONE', #14090, #6934, #903 ) ;
#1756 = CIRCLE ( 'NONE', #5285, 1.700000000000007061 ) ;
#1757 = DIRECTION ( 'NONE',  ( 0.000000000000000000, 0.000000000000000000, -1.000000000000000000 ) ) ;
#1758 = CARTESIAN_POINT ( 'NONE',  ( 175.9483885134608272, 15.03993994372673804, 24.94742576086838781 ) ) ;
#1759 = DIRECTION ( 'NONE',  ( 1.000000000000000000, 0.000000000000000000, 0.000000000000000000 ) ) ;
#1760 = VECTOR ( 'NONE', #5317, 1000.000000000000000 ) ;
#1761 = PLANE ( 'NONE',  #2765 ) ;
#1762 = CIRCLE ( 'NONE', #10603, 0.5000000000000004441 ) ;
#1763 = EDGE_LOOP ( 'NONE', ( #6689, #9777, #2063, #3637, #11582, #11850 ) ) ;
#1764 = EDGE_CURVE ( 'NONE', #10201, #15193, #1762, .T. ) ;
#1765 = CARTESIAN_POINT ( 'NONE',  ( -133.4717610386620095, 107.2638826318553953, 0.000000000000000000 ) ) ;
#1766 = CIRCLE ( 'NONE', #10604, 0.4999999999999996114 ) ;
#1767 = CARTESIAN_POINT ( 'NONE',  ( -194.3489852843322581, 137.1051365066642234, -4.640918829492427733 ) ) ;
#1768 = CARTESIAN_POINT ( 'NONE',  ( 184.0000000000000568, 17.53993994372673981, -10.99999999999999822 ) ) ;
#1769 = ORIENTED_EDGE ( 'NONE', *, *, #4176, .F. ) ;
#1770 = CARTESIAN_POINT ( 'NONE',  ( -205.9652191273047777, 131.2378527988410326, 1.515400478619091329 ) ) ;
#1771 = CARTESIAN_POINT ( 'NONE',  ( 207.2666510146856069, 31.35441966018789728, -3.370316356820458381 ) ) ;
#1772 = EDGE_LOOP ( 'NONE', ( #14110, #1416, #2018, #11573, #13939 ) ) ;
#1773 = CARTESIAN_POINT ( 'NONE',  ( 164.0000000000000568, 64.51493994372674479, 11.50000000000000000 ) ) ;
#1774 = DIRECTION ( 'NONE',  ( 0.000000000000000000, 0.000000000000000000, 1.000000000000000000 ) ) ;
#1775 = CIRCLE ( 'NONE', #12365, 0.5000000000000000000 ) ;
#1776 = DIRECTION ( 'NONE',  ( 0.000000000000000000, 0.000000000000000000, 1.000000000000000000 ) ) ;
#1777 = CIRCLE ( 'NONE', #5065, 1.499999999999997780 ) ;
#1778 = EDGE_CURVE ( 'NONE', #858, #4152, #11112, .T. ) ;
#1779 = CARTESIAN_POINT ( 'NONE',  ( 21.71949999999999648, 1.836970198721030181E-16, -1.500000000000000222 ) ) ;
#1780 = VERTEX_POINT ( 'NONE', #7055 ) ;
#1781 = CARTESIAN_POINT ( 'NONE',  ( 172.5293059057019889, 61.25683321636181233, 10.00000000000000178 ) ) ;
#1782 = CARTESIAN_POINT ( 'NONE',  ( -204.9546745879972889, 133.0893851581147374, 7.918248976830629893 ) ) ;
#1783 = CARTESIAN_POINT ( 'NONE',  ( 13.91029453487719181, 40.04259805664093363, 7.600000000000002309 ) ) ;
#1784 = CARTESIAN_POINT ( 'NONE',  ( -156.5388943062064584, 111.1998600659882896, -4.950241352008077023 ) ) ;
#1785 = VERTEX_POINT ( 'NONE', #3412 ) ;
#1787 = CARTESIAN_POINT ( 'NONE',  ( 66.76535645333922275, 38.79159067395544014, 10.00000000000000178 ) ) ;
#1786 = AXIS2_PLACEMENT_3D ( 'NONE', #554, #15078, #1828 ) ;
#1788 = ORIENTED_EDGE ( 'NONE', *, *, #7310, .T. ) ;
#1789 = ORIENTED_EDGE ( 'NONE', *, *, #14718, .T. ) ;
#1790 = DIRECTION ( 'NONE',  ( -3.965082230804130220E-16, 0.000000000000000000, -1.000000000000000000 ) ) ;
#1791 = DIRECTION ( 'NONE',  ( 0.000000000000000000, 0.000000000000000000, -1.000000000000000000 ) ) ;
#1792 = SURFACE_STYLE_FILL_AREA ( #5434 ) ;
#1793 = CARTESIAN_POINT ( 'NONE',  ( -174.2824251065520968, 115.9783496305641535, 2.177446462082195389 ) ) ;
#1794 = CARTESIAN_POINT ( 'NONE',  ( -217.7719644788709559, 153.0191138716839134, -2.888063911326615774 ) ) ;
#1795 = EDGE_CURVE ( 'NONE', #8082, #15155, #1002, .T. ) ;
#1797 = EDGE_CURVE ( 'NONE', #14752, #6214, #9094, .T. ) ;
#1796 = EDGE_CURVE ( 'NONE', #4264, #8395, #6075, .T. ) ;
#1798 = CARTESIAN_POINT ( 'NONE',  ( 177.5000000000000853, 15.03993994372673804, 38.07518420361041933 ) ) ;
#1799 = AXIS2_PLACEMENT_3D ( 'NONE', #10657, #13006, #14345 ) ;
#1800 = CARTESIAN_POINT ( 'NONE',  ( -133.4717610386620095, 107.2638826318553953, 5.000000000000000000 ) ) ;
#1801 = CIRCLE ( 'NONE', #15143, 3.500000000000003109 ) ;
#1802 = FACE_OUTER_BOUND ( 'NONE', #3961, .T. ) ;
#1803 = CARTESIAN_POINT ( 'NONE',  ( 191.4227524587821279, 39.61567282607229856, -2.929995994935606252 ) ) ;
#1804 = DIRECTION ( 'NONE',  ( 0.000000000000000000, 1.000000000000000000, 0.000000000000000000 ) ) ;
#1805 = ORIENTED_EDGE ( 'NONE', *, *, #4140, .T. ) ;
#1806 = CARTESIAN_POINT ( 'NONE',  ( -221.2434695521093602, 150.8468077239669753, 9.749916661835451137 ) ) ;
#1807 = VERTEX_POINT ( 'NONE', #12795 ) ;
#1808 = DIRECTION ( 'NONE',  ( -1.000000000000000000, -2.751328491981765035E-32, 3.965082230804130220E-16 ) ) ;
#1809 = VERTEX_POINT ( 'NONE', #11711 ) ;
#1810 = DIRECTION ( 'NONE',  ( -0.7900120431063429871, 0.6130913241491365850, 0.000000000000000000 ) ) ;
#1811 = CARTESIAN_POINT ( 'NONE',  ( 173.2749560924322907, 69.96037208313981637, -0.9107274384406881529 ) ) ;
#1812 = CIRCLE ( 'NONE', #6623, 3.499999999999996003 ) ;
#1813 = CARTESIAN_POINT ( 'NONE',  ( 177.5000000000000853, -179.8058001507315566, -51.45141194869119516 ) ) ;
#1814 = EDGE_LOOP ( 'NONE', ( #8734, #6895, #10209, #9391 ) ) ;
#1815 = CONTEXT_DEPENDENT_SHAPE_REPRESENTATION ( #1898, #10166 ) ;
#1816 = AXIS2_PLACEMENT_3D ( 'NONE', #3969, #8888, #13595 ) ;
#1817 = ORIENTED_EDGE ( 'NONE', *, *, #7244, .F. ) ;
#1818 = CARTESIAN_POINT ( 'NONE',  ( 207.3157014670556748, 31.37515976295564357, -6.367693553816072161 ) ) ;
#1819 = CARTESIAN_POINT ( 'NONE',  ( 178.0000000000000853, 15.03993994372673981, -3.075184203610571654 ) ) ;
#1820 = ORIENTED_EDGE ( 'NONE', *, *, #9243, .T. ) ;
#1822 = MECHANICAL_DESIGN_GEOMETRIC_PRESENTATION_REPRESENTATION (  '', ( #4599 ), #12887 ) ;
#1821 = AXIS2_PLACEMENT_3D ( 'NONE', #5536, #6883, #15294 ) ;
#1823 = DIRECTION ( 'NONE',  ( -5.518327896226364679E-17, 0.9902680687415713612, -0.1391731009600582492 ) ) ;
#1824 = CARTESIAN_POINT ( 'NONE',  ( 0.1708300674639756100, -3.045886356309197573, -0.2243700767916258776 ) ) ;
#1825 = ORIENTED_EDGE ( 'NONE', *, *, #7680, .F. ) ;
#1826 = ORIENTED_EDGE ( 'NONE', *, *, #4772, .T. ) ;
#1827 = CARTESIAN_POINT ( 'NONE',  ( 10.39230484541326582, 0.000000000000000000, 0.000000000000000000 ) ) ;
#1828 = DIRECTION ( 'NONE',  ( 0.000000000000000000, 0.000000000000000000, 1.000000000000000000 ) ) ;
#1829 = EDGE_CURVE ( 'NONE', #4912, #5662, #3336, .T. ) ;
#1830 = EDGE_LOOP ( 'NONE', ( #15345, #10863, #12246, #390 ) ) ;
#1831 = CARTESIAN_POINT ( 'NONE',  ( 0.08224679563971951102, -6.145890662064638299, 5.355005115540925509 ) ) ;
#1832 = DIRECTION ( 'NONE',  ( 0.000000000000000000, -0.000000000000000000, -1.000000000000000000 ) ) ;
#1833 = CARTESIAN_POINT ( 'NONE',  ( -110.0000000000000426, 22.53993994372673981, 24.99999999999999645 ) ) ;
#1834 = DIRECTION ( 'NONE',  ( 0.000000000000000000, 0.000000000000000000, -1.000000000000000000 ) ) ;
#1835 = DIRECTION ( 'NONE',  ( -0.000000000000000000, -0.000000000000000000, 1.000000000000000000 ) ) ;
#1836 = VECTOR ( 'NONE', #7426, 999.9999999999997726 ) ;
#1837 = CYLINDRICAL_SURFACE ( 'NONE', #3271, 1.699999999999996625 ) ;
#1838 = VERTEX_POINT ( 'NONE', #9266 ) ;
#1839 = DIRECTION ( 'NONE',  ( 0.4873681696970814103, 0.8731965799097685110, 0.000000000000000000 ) ) ;
#1840 = CARTESIAN_POINT ( 'NONE',  ( -218.4400809351218413, 155.8695184890967482, 1.515441477806783510 ) ) ;
#1841 = CARTESIAN_POINT ( 'NONE',  ( 178.0000000000000853, 15.53993994372673981, 25.38206912977650376 ) ) ;
#1842 = ORIENTED_EDGE ( 'NONE', *, *, #14993, .F. ) ;
#1843 = CARTESIAN_POINT ( 'NONE',  ( -213.9961813491638623, 134.6717504882919911, 1.515400478619087776 ) ) ;
#1844 = CARTESIAN_POINT ( 'NONE',  ( 198.4239224672526234, 29.08807987246144933, -3.746314016867685837 ) ) ;
#1845 = VECTOR ( 'NONE', #11518, 1000.000000000000000 ) ;
#1846 = EDGE_LOOP ( 'NONE', ( #10498, #6434, #10055, #11627, #4626, #13978 ) ) ;
#1847 = AXIS2_PLACEMENT_3D ( 'NONE', #5513, #3933, #8755 ) ;
#1848 = CARTESIAN_POINT ( 'NONE',  ( 0.1090894304641079615, 2.915265454974091064, 0.4506121144344771290 ) ) ;
#1849 = DIRECTION ( 'NONE',  ( -1.000000000000000000, 0.000000000000000000, 0.000000000000000000 ) ) ;
#1850 = EDGE_CURVE ( 'NONE', #15505, #12940, #4802, .T. ) ;
#1851 = DIRECTION ( 'NONE',  ( 0.000000000000000000, 0.9569673715906176215, 0.2901955370279575286 ) ) ;
#1852 = AXIS2_PLACEMENT_3D ( 'NONE', #4069, #8904, #3849 ) ;
#1853 = CARTESIAN_POINT ( 'NONE',  ( -76.00000000000004263, 15.03993994372673804, 38.07518420361041933 ) ) ;
#1854 = ORIENTED_EDGE ( 'NONE', *, *, #11944, .T. ) ;
#1855 = DIRECTION ( 'NONE',  ( 0.000000000000000000, 0.000000000000000000, -1.000000000000000000 ) ) ;
#1856 = CARTESIAN_POINT ( 'NONE',  ( -218.3193879687431433, 147.6986783750013217, 10.16010209732750980 ) ) ;
#1857 = CARTESIAN_POINT ( 'NONE',  ( 190.0000000000000853, 16.03993994372673626, 38.07518420361041933 ) ) ;
#1858 = DIRECTION ( 'NONE',  ( 1.000000000000000000, 0.000000000000000000, 0.000000000000000000 ) ) ;
#1859 = EDGE_LOOP ( 'NONE', ( #2042, #2199, #11914, #1842 ) ) ;
#1860 = LINE ( 'NONE', #2178, #9876 ) ;
#1861 = EDGE_CURVE ( 'NONE', #12197, #8972, #3037, .T. ) ;
#1862 = ORIENTED_EDGE ( 'NONE', *, *, #6839, .F. ) ;
#1863 = EDGE_LOOP ( 'NONE', ( #13669, #11225 ) ) ;
#1864 = LINE ( 'NONE', #15347, #13706 ) ;
#1865 = DIRECTION ( 'NONE',  ( 0.000000000000000000, -6.938893903907222067E-15, 1.000000000000000000 ) ) ;
#1866 = VECTOR ( 'NONE', #14338, 1000.000000000000000 ) ;
#1867 = DIRECTION ( 'NONE',  ( -0.8731965799097679559, 0.4873681696970824095, 0.000000000000000000 ) ) ;
#1868 = CARTESIAN_POINT ( 'NONE',  ( -167.8057708040753653, 127.5822924766788447, 2.966601681492425868 ) ) ;
#1869 = CARTESIAN_POINT ( 'NONE',  ( -217.8572871788818475, 152.8680898606328356, -3.058345895658412417 ) ) ;
#1870 = CARTESIAN_POINT ( 'NONE',  ( -70.00000000000000000, 17.53993994372673981, -13.99999999999999112 ) ) ;
#1871 = CARTESIAN_POINT ( 'NONE',  ( -76.00000000000001421, -178.8058001507315566, 52.19066787724494816 ) ) ;
#1872 = PRODUCT_DEFINITION_CONTEXT ( 'detailed design', #785, 'design' ) ;
#1873 = CARTESIAN_POINT ( 'NONE',  ( 174.2293059057019775, 61.25683321636181233, 5.000000000000000000 ) ) ;
#1874 = EDGE_CURVE ( 'NONE', #10895, #14008, #4279, .T. ) ;
#1875 = DIRECTION ( 'NONE',  ( 1.000000000000000000, 0.000000000000000000, 0.000000000000000000 ) ) ;
#1876 = DIRECTION ( 'NONE',  ( 1.000000000000000000, 0.000000000000000000, 0.000000000000000000 ) ) ;
#1877 = ORIENTED_EDGE ( 'NONE', *, *, #5337, .T. ) ;
#1878 = ADVANCED_FACE ( 'NONE', ( #12879 ), #4591, .F. ) ;
#1879 = VERTEX_POINT ( 'NONE', #11634 ) ;
#1880 = EDGE_CURVE ( 'NONE', #10586, #12024, #6900, .T. ) ;
#1881 = CARTESIAN_POINT ( 'NONE',  ( -174.1255661870616507, 116.2593870075281473, -0.1232875569927439491 ) ) ;
#1882 = DIRECTION ( 'NONE',  ( -0.9951762285753402715, 0.09810338464376280876, -0.000000000000000000 ) ) ;
#1883 = CARTESIAN_POINT ( 'NONE',  ( -108.0000000000000568, 64.53993994372673626, 10.00000000000000178 ) ) ;
#1884 = CARTESIAN_POINT ( 'NONE',  ( -157.6477983077465694, 110.1970436846184924, 9.411501811869198875 ) ) ;
#1885 = CARTESIAN_POINT ( 'NONE',  ( -76.00000000000001421, 16.03993994372673981, -7.458121719691109004E-14 ) ) ;
#1886 = EDGE_CURVE ( 'NONE', #8972, #935, #795, .T. ) ;
#1887 = VECTOR ( 'NONE', #7298, 1000.000000000000000 ) ;
#1888 = CARTESIAN_POINT ( 'NONE',  ( 122.5806775638430253, 45.00321902537314145, 0.000000000000000000 ) ) ;
#1889 = ORIENTED_EDGE ( 'NONE', *, *, #13553, .F. ) ;
#1890 = APPLICATION_PROTOCOL_DEFINITION ( 'draft international standard', 'automotive_design', 1998, #15611 ) ;
#1891 = ORIENTED_EDGE ( 'NONE', *, *, #15273, .T. ) ;
#1892 = CARTESIAN_POINT ( 'NONE',  ( 201.6895650671498288, 29.08490409614774208, -0.6212496039192949571 ) ) ;
#1893 = CARTESIAN_POINT ( 'NONE',  ( 0.000000000000000000, 15.53993994372673981, 7.305634244248866343E-16 ) ) ;
#1894 = EDGE_LOOP ( 'NONE', ( #11736, #12320, #155 ) ) ;
#1895 = FACE_OUTER_BOUND ( 'NONE', #5225, .T. ) ;
#1896 = VECTOR ( 'NONE', #5151, 999.9999999999998863 ) ;
#1897 = EDGE_CURVE ( 'NONE', #7467, #12599, #1513, .T. ) ;
#1899 = ADVANCED_FACE ( 'NONE', ( #14214 ), #11863, .F. ) ;
#1898 =( REPRESENTATION_RELATIONSHIP ('NONE','NONE', #3298, #8648 ) REPRESENTATION_RELATIONSHIP_WITH_TRANSFORMATION ( #6886 )SHAPE_REPRESENTATION_RELATIONSHIP( ) );
#1900 = CARTESIAN_POINT ( 'NONE',  ( -156.6477983077465410, 110.1970436846185066, 84.88378295107887084 ) ) ;
#1901 = EDGE_LOOP ( 'NONE', ( #1292, #1740, #6793, #7476 ) ) ;
#1902 = ORIENTED_EDGE ( 'NONE', *, *, #4463, .T. ) ;
#1903 = CARTESIAN_POINT ( 'NONE',  ( 172.5293059057019889, 61.25683321636181233, 7.600000000000002309 ) ) ;
#1904 = DIRECTION ( 'NONE',  ( 0.000000000000000000, 1.000000000000000000, 6.938893903907227145E-17 ) ) ;
#1905 = ORIENTED_EDGE ( 'NONE', *, *, #10039, .T. ) ;
#1906 = CARTESIAN_POINT ( 'NONE',  ( 205.4339596421060889, 33.86846485884471747, -4.932823326473320336 ) ) ;
#1907 = LINE ( 'NONE', #2222, #12357 ) ;
#1908 = EDGE_CURVE ( 'NONE', #8130, #2947, #1907, .T. ) ;
#1909 = CARTESIAN_POINT ( 'NONE',  ( 64.00000000000005684, 64.51493994372674479, 18.50000000000070344 ) ) ;
#1910 = DIRECTION ( 'NONE',  ( 0.000000000000000000, 0.000000000000000000, 1.000000000000000000 ) ) ;
#1911 = CARTESIAN_POINT ( 'NONE',  ( 184.0000000000000568, 17.53993994372673271, 47.49999999999997868 ) ) ;
#1912 = ADVANCED_FACE ( 'NONE', ( #10679, #15472, #4668 ), #13915, .T. ) ;
#1913 = VECTOR ( 'NONE', #13223, 1000.000000000000000 ) ;
#1914 = CARTESIAN_POINT ( 'NONE',  ( 177.5000000000000853, 14.90076684276667862, -2.084916134868993076 ) ) ;
#1915 = EDGE_LOOP ( 'NONE', ( #530, #360, #10507, #9850, #14863, #4420 ) ) ;
#1916 = FACE_OUTER_BOUND ( 'NONE', #13980, .T. ) ;
#1917 = CARTESIAN_POINT ( 'NONE',  ( -174.7802519396333878, 131.5011100042426904, 1.515441477806783066 ) ) ;
#1918 = CARTESIAN_POINT ( 'NONE',  ( 70.26535645333922275, 38.79159067395544014, 0.000000000000000000 ) ) ;
#1919 = ORIENTED_EDGE ( 'NONE', *, *, #7073, .F. ) ;
#1920 = CARTESIAN_POINT ( 'NONE',  ( -178.4115273750087738, 119.2860570028907858, -3.078262048313290311 ) ) ;
#1921 = CARTESIAN_POINT ( 'NONE',  ( 209.6393851568315938, 47.95822392590527983, 0.3767681043515945238 ) ) ;
#1922 = ORIENTED_EDGE ( 'NONE', *, *, #4578, .F. ) ;
#1923 = FACE_BOUND ( 'NONE', #2485, .T. ) ;
#1924 = DIRECTION ( 'NONE',  ( -0.000000000000000000, 1.000000000000000000, -0.000000000000000000 ) ) ;
#1925 = CARTESIAN_POINT ( 'NONE',  ( -150.6072264393035027, 106.6613139020875423, -4.675203989473062371 ) ) ;
#1926 = EDGE_CURVE ( 'NONE', #830, #3704, #9593, .T. ) ;
#1927 = DIRECTION ( 'NONE',  ( 0.9956600981502441439, -0.09306432695424331214, 0.000000000000000000 ) ) ;
#1928 = CARTESIAN_POINT ( 'NONE',  ( 0.000000000000000000, 19.53993994372674337, 2.905405074819403421E-15 ) ) ;
#1929 = EDGE_CURVE ( 'NONE', #10201, #12658, #2383, .T. ) ;
#1930 = EDGE_LOOP ( 'NONE', ( #13294, #7913, #5232, #9705, #8762, #1514 ) ) ;
#1931 = DIRECTION ( 'NONE',  ( 0.000000000000000000, 2.775557561562888827E-14, 1.000000000000000000 ) ) ;
#1932 = CARTESIAN_POINT ( 'NONE',  ( -170.7405378081422214, 121.6209906574826931, 10.02899269843361374 ) ) ;
#1933 = CARTESIAN_POINT ( 'NONE',  ( 14.00000000000004086, 64.53993994372673626, 15.00000000000104983 ) ) ;
#1934 = LINE ( 'NONE', #11506, #11849 ) ;
#1935 = ORIENTED_EDGE ( 'NONE', *, *, #8976, .T. ) ;
#1936 = DIRECTION ( 'NONE',  ( 1.000000000000000000, -2.751328491981765035E-32, 3.965082230804130220E-16 ) ) ;
#1937 = ORIENTED_EDGE ( 'NONE', *, *, #4142, .F. ) ;
#1938 = EDGE_LOOP ( 'NONE', ( #2435, #14717, #9875, #7857 ) ) ;
#1939 = DIRECTION ( 'NONE',  ( 3.965082230804130220E-16, -1.486905836551548832E-16, 1.000000000000000000 ) ) ;
#1940 = CARTESIAN_POINT ( 'NONE',  ( 14.00000000000004086, 64.53993994372673626, 11.50000000000105160 ) ) ;
#1941 = DIRECTION ( 'NONE',  ( 0.000000000000000000, 0.000000000000000000, 1.000000000000000000 ) ) ;
#1942 = CARTESIAN_POINT ( 'NONE',  ( -173.2932605743736474, 117.7505931626010778, 7.695635371731032848 ) ) ;
#1943 = CARTESIAN_POINT ( 'NONE',  ( -222.5489981585923545, 148.5077482920355862, -5.007338236124175168 ) ) ;
#1944 = CARTESIAN_POINT ( 'NONE',  ( 190.0000000000000568, -178.7362136002515172, -17.68580191161595394 ) ) ;
#1945 = LINE ( 'NONE', #5518, #1845 ) ;
#1946 = FACE_OUTER_BOUND ( 'NONE', #9084, .T. ) ;
#1947 = EDGE_CURVE ( 'NONE', #11858, #256, #2789, .T. ) ;
#1948 = CARTESIAN_POINT ( 'NONE',  ( -61.94838851346079167, -179.3058001507315566, -51.45141194869120227 ) ) ;
#1949 = VECTOR ( 'NONE', #2753, 1000.000000000000114 ) ;
#1950 = CARTESIAN_POINT ( 'NONE',  ( 177.5000000000000853, -179.8058001507315566, 84.88378295107887084 ) ) ;
#1951 = LINE ( 'NONE', #12531, #33 ) ;
#1952 = EDGE_LOOP ( 'NONE', ( #167, #14824, #4080, #14115, #2555, #13580, #2871, #3149 ) ) ;
#1953 = CONICAL_SURFACE ( 'NONE', #14548, 3.524999999999998579, 0.7853981633974482790 ) ;
#1954 =( NAMED_UNIT ( * ) SI_UNIT ( $, .STERADIAN. ) SOLID_ANGLE_UNIT ( ) );
#1955 = VERTEX_POINT ( 'NONE', #12015 ) ;
#1956 = CARTESIAN_POINT ( 'NONE',  ( 178.0000000000000853, -178.8058001507315566, -17.19066787724516843 ) ) ;
#1957 = FACE_OUTER_BOUND ( 'NONE', #577, .T. ) ;
#1958 = ORIENTED_EDGE ( 'NONE', *, *, #11334, .T. ) ;
#1959 = CYLINDRICAL_SURFACE ( 'NONE', #13197, 1.699999999999993072 ) ;
#1960 = LINE ( 'NONE', #6798, #8102 ) ;
#1961 = PRODUCT_DEFINITION_SHAPE ( 'NONE', 'NONE',  #15626 ) ;
#1962 = ADVANCED_FACE ( 'NONE', ( #8477 ), #1111, .F. ) ;
#1963 = AXIS2_PLACEMENT_3D ( 'NONE', #9341, #14136, #11472 ) ;
#1964 = DIRECTION ( 'NONE',  ( 0.000000000000000000, 0.000000000000000000, 1.000000000000000000 ) ) ;
#1965 = ORIENTED_EDGE ( 'NONE', *, *, #9339, .F. ) ;
#1966 = AXIS2_PLACEMENT_3D ( 'NONE', #11193, #14569, #3770 ) ;
#1967 = EDGE_CURVE ( 'NONE', #5844, #1807, #3233, .T. ) ;
#1968 = SHAPE_DEFINITION_REPRESENTATION ( #564, #8648 ) ;
#1969 = ORIENTED_EDGE ( 'NONE', *, *, #12096, .T. ) ;
#1970 = CARTESIAN_POINT ( 'NONE',  ( 207.2819921120892275, 50.35227183911742088, -8.638656677529437999 ) ) ;
#1971 = CYLINDRICAL_SURFACE ( 'NONE', #523, 1.700000000000007061 ) ;
#1972 = ORIENTED_EDGE ( 'NONE', *, *, #10428, .T. ) ;
#1973 = CARTESIAN_POINT ( 'NONE',  ( 178.0000000000000853, 15.53993994372673981, 10.05257423913146475 ) ) ;
#1974 = AXIS2_PLACEMENT_3D ( 'NONE', #14287, #2218, #11936 ) ;
#1975 = DIRECTION ( 'NONE',  ( 1.000000000000000000, 0.000000000000000000, 0.000000000000000000 ) ) ;
#1976 = ORIENTED_EDGE ( 'NONE', *, *, #7499, .F. ) ;
#1977 = ORIENTED_EDGE ( 'NONE', *, *, #15100, .F. ) ;
#1978 = LINE ( 'NONE', #633, #12056 ) ;
#1979 = DIRECTION ( 'NONE',  ( 0.000000000000000000, 0.000000000000000000, -1.000000000000000000 ) ) ;
#1980 = AXIS2_PLACEMENT_3D ( 'NONE', #6052, #11021, #9683 ) ;
#1981 = ORIENTED_EDGE ( 'NONE', *, *, #8820, .F. ) ;
#1982 = CARTESIAN_POINT ( 'NONE',  ( 0.3173508448886587785, -5.375634714784612633, 6.689127551062028942 ) ) ;
#1983 = DIRECTION ( 'NONE',  ( -0.000000000000000000, -0.000000000000000000, 1.000000000000000000 ) ) ;
#1984 = DIRECTION ( 'NONE',  ( 0.000000000000000000, 0.000000000000000000, 1.000000000000000000 ) ) ;
#1985 = DIRECTION ( 'NONE',  ( -1.000000000000000000, -0.000000000000000000, -0.000000000000000000 ) ) ;
#1986 = DIRECTION ( 'NONE',  ( 1.000000000000000000, -2.751328491981765035E-32, 3.965082230804130220E-16 ) ) ;
#1987 = ADVANCED_FACE ( 'NONE', ( #6101 ), #7291, .F. ) ;
#1988 = EDGE_CURVE ( 'NONE', #10586, #5590, #12098, .T. ) ;
#1989 = EDGE_CURVE ( 'NONE', #2929, #13434, #7442, .T. ) ;
#1990 = AXIS2_PLACEMENT_3D ( 'NONE', #15444, #3390, #13315 ) ;
#1991 = AXIS2_PLACEMENT_3D ( 'NONE', #12249, #3815, #2554 ) ;
#1992 = DIRECTION ( 'NONE',  ( 1.000000000000000000, 0.000000000000000000, 0.000000000000000000 ) ) ;
#1993 = ORIENTED_EDGE ( 'NONE', *, *, #15375, .F. ) ;
#1994 = DIRECTION ( 'NONE',  ( 0.000000000000000000, 0.000000000000000000, 1.000000000000000000 ) ) ;
#1995 = CARTESIAN_POINT ( 'NONE',  ( -206.0135413368010404, 148.9337379340180405, 1.515441477536285220 ) ) ;
#1996 = DIRECTION ( 'NONE',  ( 0.000000000000000000, 0.1391731009600582492, 0.9902680687415713612 ) ) ;
#1997 = EDGE_LOOP ( 'NONE', ( #2216, #13119, #7159, #10044 ) ) ;
#1998 = CARTESIAN_POINT ( 'NONE',  ( -190.6388552492889517, 127.3288340616119143, -2.964974570226841522 ) ) ;
#1999 = CARTESIAN_POINT ( 'NONE',  ( 198.5423134874356208, 52.64753739496011065, -2.122073255223759780 ) ) ;
#2000 = CIRCLE ( 'NONE', #10341, 8.000000000000028422 ) ;
#2001 = EDGE_LOOP ( 'NONE', ( #3858, #3321, #12575, #4549 ) ) ;
#2002 = AXIS2_PLACEMENT_3D ( 'NONE', #2956, #8720, #7775 ) ;
#2003 = EDGE_CURVE ( 'NONE', #8877, #652, #12086, .T. ) ;
#2004 = CARTESIAN_POINT ( 'NONE',  ( -70.00000000000000000, 17.53993994372673981, -10.99999999999999822 ) ) ;
#2005 = FACE_OUTER_BOUND ( 'NONE', #9338, .T. ) ;
#2006 = DIRECTION ( 'NONE',  ( 0.000000000000000000, -1.000000000000000000, 0.000000000000000000 ) ) ;
#2007 = ORIENTED_EDGE ( 'NONE', *, *, #2102, .T. ) ;
#2008 = DIRECTION ( 'NONE',  ( 2.117253093321598312E-15, -3.584345385556270492E-16, 1.000000000000000000 ) ) ;
#2009 = AXIS2_PLACEMENT_3D ( 'NONE', #7353, #9634, #6085 ) ;
#2010 = DIRECTION ( 'NONE',  ( 1.000000000000000000, 0.000000000000000000, 0.000000000000000000 ) ) ;
#2011 = ORIENTED_EDGE ( 'NONE', *, *, #6190, .T. ) ;
#2012 = CARTESIAN_POINT ( 'NONE',  ( -63.50000000000002842, -178.8058001507315566, -17.19066787724516843 ) ) ;
#2013 = CARTESIAN_POINT ( 'NONE',  ( -216.0863581598438543, 143.0557482234525253, 9.577123744044239828 ) ) ;
#2014 = FACE_OUTER_BOUND ( 'NONE', #8148, .T. ) ;
#2015 = CYLINDRICAL_SURFACE ( 'NONE', #11093, 0.5000000000000004441 ) ;
#2016 = ORIENTED_EDGE ( 'NONE', *, *, #6082, .T. ) ;
#2017 = DIRECTION ( 'NONE',  ( -0.000000000000000000, 0.1391731009600582492, 0.9902680687415713612 ) ) ;
#2018 = ORIENTED_EDGE ( 'NONE', *, *, #4319, .F. ) ;
#2019 = ADVANCED_FACE ( 'NONE', ( #9731 ), #6016, .T. ) ;
#2020 = ORIENTED_EDGE ( 'NONE', *, *, #1479, .F. ) ;
#2021 = VECTOR ( 'NONE', #6436, 1000.000000000000114 ) ;
#2022 = CARTESIAN_POINT ( 'NONE',  ( 0.7145311798163155315, -4.618802153516981868, 8.000000000000007105 ) ) ;
#2023 = DIRECTION ( 'NONE',  ( 0.000000000000000000, -1.000000000000000000, 0.000000000000000000 ) ) ;
#2024 = CIRCLE ( 'NONE', #1525, 1.700000000000001954 ) ;
#2025 = EDGE_CURVE ( 'NONE', #3026, #5369, #6087, .T. ) ;
#2026 = VECTOR ( 'NONE', #12664, 1000.000000000000000 ) ;
#2027 = DIRECTION ( 'NONE',  ( 0.000000000000000000, 0.1391731009600592484, 0.9902680687415712502 ) ) ;
#2028 = CARTESIAN_POINT ( 'NONE',  ( 175.9483885134608272, -179.3058001507315566, -51.45141194869120227 ) ) ;
#2029 = CARTESIAN_POINT ( 'NONE',  ( -224.6670067989573454, 144.7130033415326977, -2.813789935910935736 ) ) ;
#2030 = CARTESIAN_POINT ( 'NONE',  ( 50.57199999999998852, 6.123233995736767268E-16, -5.000000000000000000 ) ) ;
#2031 = PLANE ( 'NONE',  #1599 ) ;
#2032 = CIRCLE ( 'NONE', #3551, 0.5000000000000004441 ) ;
#2033 = CARTESIAN_POINT ( 'NONE',  ( 70.26535645333922275, 38.79159067395544014, 5.000000000000000000 ) ) ;
#2034 = CIRCLE ( 'NONE', #13636, 3.752352628381527833 ) ;
#2035 = DIRECTION ( 'NONE',  ( 1.504267769033196424E-15, 0.9902680687415713612, 0.1391731009600591373 ) ) ;
#2036 = CARTESIAN_POINT ( 'NONE',  ( 51.39999999999999858, 0.000000000000000000, 4.172000000000013920 ) ) ;
#2037 = ORIENTED_EDGE ( 'NONE', *, *, #5828, .F. ) ;
#2038 = EDGE_LOOP ( 'NONE', ( #12635, #8168, #11069, #1650 ) ) ;
#2039 = EDGE_CURVE ( 'NONE', #7454, #8789, #10609, .T. ) ;
#2040 = FACE_OUTER_BOUND ( 'NONE', #13110, .T. ) ;
#2041 = DIRECTION ( 'NONE',  ( 0.000000000000000000, 0.000000000000000000, -1.000000000000000000 ) ) ;
#2042 = ORIENTED_EDGE ( 'NONE', *, *, #1947, .F. ) ;
#2043 = DIRECTION ( 'NONE',  ( 3.965082230804130220E-16, 1.090924371466202084E-47, 1.000000000000000000 ) ) ;
#2044 = DIRECTION ( 'NONE',  ( -0.000000000000000000, 1.000000000000000000, -0.000000000000000000 ) ) ;
#2045 = VECTOR ( 'NONE', #14822, 1000.000000000000000 ) ;
#2046 = FACE_OUTER_BOUND ( 'NONE', #7317, .T. ) ;
#2048 = ORIENTED_EDGE ( 'NONE', *, *, #14989, .F. ) ;
#2047 = EDGE_CURVE ( 'NONE', #11935, #4694, #4914, .T. ) ;
#2049 = VERTEX_POINT ( 'NONE', #10994 ) ;
#2050 = CARTESIAN_POINT ( 'NONE',  ( 207.5020891771285960, 50.23084475345794431, 0.4952462535581279024 ) ) ;
#2051 = EDGE_CURVE ( 'NONE', #5037, #299, #9803, .T. ) ;
#2052 = ORIENTED_EDGE ( 'NONE', *, *, #10291, .T. ) ;
#2053 = CARTESIAN_POINT ( 'NONE',  ( 6.800000000000000711, 0.000000000000000000, 0.000000000000000000 ) ) ;
#2054 = AXIS2_PLACEMENT_3D ( 'NONE', #12743, #5498, #15107 ) ;
#2055 = DIRECTION ( 'NONE',  ( -0.000000000000000000, 1.000000000000000000, -0.000000000000000000 ) ) ;
#2056 = DIRECTION ( 'NONE',  ( 0.000000000000000000, 0.000000000000000000, -1.000000000000000000 ) ) ;
#2057 = ORIENTED_EDGE ( 'NONE', *, *, #6303, .F. ) ;
#2058 = ORIENTED_EDGE ( 'NONE', *, *, #6781, .F. ) ;
#2059 = AXIS2_PLACEMENT_3D ( 'NONE', #15441, #9540, #845 ) ;
#2060 = CARTESIAN_POINT ( 'NONE',  ( -76.50000000000001421, -178.8058001507315566, -17.19066787724516843 ) ) ;
#2061 = FACE_BOUND ( 'NONE', #14693, .T. ) ;
#2062 = EDGE_CURVE ( 'NONE', #6505, #10500, #2539, .T. ) ;
#2063 = ORIENTED_EDGE ( 'NONE', *, *, #7722, .F. ) ;
#2064 = CYLINDRICAL_SURFACE ( 'NONE', #15551, 0.5000000000000004441 ) ;
#2065 = CARTESIAN_POINT ( 'NONE',  ( -76.00000000000001421, 16.03993994372673981, 10.05257423913146475 ) ) ;
#2066 = ADVANCED_BREP_SHAPE_REPRESENTATION ( '', ( #5622, #12337 ), #10297 ) ;
#2067 = DIRECTION ( 'NONE',  ( 0.000000000000000000, 0.000000000000000000, 1.000000000000000000 ) ) ;
#2068 = CARTESIAN_POINT ( 'NONE',  ( -70.00000000000000000, 17.53993994372673626, 47.49999999999997868 ) ) ;
#2069 = B_SPLINE_CURVE_WITH_KNOTS ( 'NONE', 3,
 ( #10264, #5683, #11450, #770, #15056, #4246, #9008, #8150 ),
 .UNSPECIFIED., .F., .F.,
 ( 4, 2, 2, 4 ),
 ( 0.004673709593152115815, 0.005837709341827616513, 0.007001709090503118078, 0.009329708587854120341 ),
 .UNSPECIFIED. ) ;
#2070 = DIRECTION ( 'NONE',  ( 0.000000000000000000, 0.000000000000000000, -1.000000000000000000 ) ) ;
#2071 = CIRCLE ( 'NONE', #7884, 0.5000000000000004441 ) ;
#2072 = VECTOR ( 'NONE', #11351, 1000.000000000000000 ) ;
#2073 = CARTESIAN_POINT ( 'NONE',  ( 64.00000000000005684, 64.53993994372673626, 15.00000000000070166 ) ) ;
#2074 = ORIENTED_EDGE ( 'NONE', *, *, #6696, .F. ) ;
#2075 = CARTESIAN_POINT ( 'NONE',  ( 200.1062858801516597, 45.86394065090266992, 12.00000000000001066 ) ) ;
#2076 = CARTESIAN_POINT ( 'NONE',  ( -199.5653198453618700, 142.9393910578133102, -2.963320117457100000 ) ) ;
#2077 = DIRECTION ( 'NONE',  ( 0.000000000000000000, -1.000000000000000000, -2.731481088613017720E-16 ) ) ;
#2078 = ORIENTED_EDGE ( 'NONE', *, *, #15014, .T. ) ;
#2079 = CARTESIAN_POINT ( 'NONE',  ( -183.9200705329474772, 121.1751083001002485, -2.964974570226829087 ) ) ;
#2080 = CARTESIAN_POINT ( 'NONE',  ( 207.2638851143210275, 31.35908548908414417, -0.3703513705075706097 ) ) ;
#2081 = ORIENTED_EDGE ( 'NONE', *, *, #916, .T. ) ;
#2082 = EDGE_CURVE ( 'NONE', #3561, #720, #11065, .T. ) ;
#2084 = EDGE_CURVE ( 'NONE', #15428, #8632, #4294, .T. ) ;
#2083 = ADVANCED_FACE ( 'NONE', ( #3484 ), #13106, .F. ) ;
#2085 = AXIS2_PLACEMENT_3D ( 'NONE', #10680, #1185, #12089 ) ;
#2086 = CARTESIAN_POINT ( 'NONE',  ( -70.00000000000000000, 19.53993994372674337, -10.99999999999999822 ) ) ;
#2087 = DIRECTION ( 'NONE',  ( 0.000000000000000000, 0.000000000000000000, 1.000000000000000000 ) ) ;
#2088 = EDGE_CURVE ( 'NONE', #7203, #4389, #11625, .T. ) ;
#2089 = VECTOR ( 'NONE', #1418, 1000.000000000000000 ) ;
#2090 = DIRECTION ( 'NONE',  ( 0.000000000000000000, 0.000000000000000000, -1.000000000000000000 ) ) ;
#2091 = ORIENTED_EDGE ( 'NONE', *, *, #3486, .F. ) ;
#2092 = CARTESIAN_POINT ( 'NONE',  ( 0.000000000000000000, 0.000000000000000000, 0.000000000000000000 ) ) ;
#2093 = DIRECTION ( 'NONE',  ( -0.000000000000000000, 1.000000000000000000, 1.486905836551548832E-16 ) ) ;
#2094 = DIRECTION ( 'NONE',  ( 0.000000000000000000, 0.000000000000000000, 1.000000000000000000 ) ) ;
#2095 = ORIENTED_EDGE ( 'NONE', *, *, #14233, .F. ) ;
#2096 = DIRECTION ( 'NONE',  ( 1.000000000000000000, 0.000000000000000000, 0.000000000000000000 ) ) ;
#2097 = VECTOR ( 'NONE', #15046, 1000.000000000000114 ) ;
#2098 = CARTESIAN_POINT ( 'NONE',  ( -212.4168668197547731, 139.5435760318306677, 9.577123744044230946 ) ) ;
#2099 = DIRECTION ( 'NONE',  ( 0.000000000000000000, 0.000000000000000000, -1.000000000000000000 ) ) ;
#2100 = CARTESIAN_POINT ( 'NONE',  ( 0.000000000000000000, 2.381569860407204420, 1.375000000000001110 ) ) ;
#2101 = DIRECTION ( 'NONE',  ( -0.000000000000000000, 1.000000000000000000, -0.000000000000000000 ) ) ;
#2102 = EDGE_CURVE ( 'NONE', #3731, #7373, #13620, .T. ) ;
#2103 = ORIENTED_EDGE ( 'NONE', *, *, #380, .F. ) ;
#2104 = ORIENTED_EDGE ( 'NONE', *, *, #14518, .T. ) ;
#2105 = FACE_OUTER_BOUND ( 'NONE', #610, .T. ) ;
#2106 = CARTESIAN_POINT ( 'NONE',  ( 114.0000000000000568, 59.53993994372674337, 15.00000000000035172 ) ) ;
#2107 = DIRECTION ( 'NONE',  ( 0.000000000000000000, 0.000000000000000000, 1.000000000000000000 ) ) ;
#2108 = CARTESIAN_POINT ( 'NONE',  ( -171.9943068686860386, 120.0778726276766122, 9.490183841837444234 ) ) ;
#2109 = CARTESIAN_POINT ( 'NONE',  ( -221.8782673190587786, 149.7094678780528909, -3.059957786404165603 ) ) ;
#2110 = AXIS2_PLACEMENT_3D ( 'NONE', #11190, #2821, #13614 ) ;
#2111 = ADVANCED_FACE ( 'NONE', ( #6334 ), #8858, .T. ) ;
#2112 = CARTESIAN_POINT ( 'NONE',  ( -218.3504703772591711, 152.0071873827878335, 8.737647451593067771 ) ) ;
#2113 = AXIS2_PLACEMENT_3D ( 'NONE', #6139, #5978, #10959 ) ;
#2114 = DIRECTION ( 'NONE',  ( -0.000000000000000000, -0.000000000000000000, -1.000000000000000000 ) ) ;
#2115 = DIRECTION ( 'NONE',  ( -1.000000000000000000, 0.000000000000000000, 0.000000000000000000 ) ) ;
#2116 = ADVANCED_FACE ( 'NONE', ( #5293 ), #1578, .F. ) ;
#2117 = DIRECTION ( 'NONE',  ( 0.000000000000000000, 1.000000000000000000, 0.000000000000000000 ) ) ;
#2118 = LINE ( 'NONE', #10726, #5858 ) ;
#2119 = ORIENTED_EDGE ( 'NONE', *, *, #10977, .T. ) ;
#2120 = VECTOR ( 'NONE', #1349, 1000.000000000000000 ) ;
#2121 = ORIENTED_EDGE ( 'NONE', *, *, #6897, .F. ) ;
#2122 = CARTESIAN_POINT ( 'NONE',  ( 19.11029453487719110, 40.04259805664093363, 5.000000000000000000 ) ) ;
#2124 = EDGE_LOOP ( 'NONE', ( #15529, #10353, #3293, #4269 ) ) ;
#2123 = STYLED_ITEM ( 'NONE', ( #4412 ), #5438 ) ;
#2125 = CARTESIAN_POINT ( 'NONE',  ( -179.9267697467775520, 134.3633106217456543, 2.500000000000000000 ) ) ;
#2126 = CARTESIAN_POINT ( 'NONE',  ( 70.26535645333922275, 38.79159067395544014, 7.600000000000002309 ) ) ;
#2127 = ORIENTED_EDGE ( 'NONE', *, *, #8471, .T. ) ;
#2128 = AXIS2_PLACEMENT_3D ( 'NONE', #13133, #3596, #10946 ) ;
#2129 = ORIENTED_EDGE ( 'NONE', *, *, #12783, .T. ) ;
#2130 = CARTESIAN_POINT ( 'NONE',  ( 188.3492591927541753, 42.47468418338397811, -7.638025320682917396 ) ) ;
#2131 = EDGE_CURVE ( 'NONE', #1137, #10552, #6843, .T. ) ;
#2132 = CARTESIAN_POINT ( 'NONE',  ( -155.6477983077465410, 110.1970436846185066, -5.000000000000000000 ) ) ;
#2133 = ORIENTED_EDGE ( 'NONE', *, *, #8002, .F. ) ;
#2134 = FACE_OUTER_BOUND ( 'NONE', #14405, .T. ) ;
#2135 = CARTESIAN_POINT ( 'NONE',  ( 0.000000000000000000, 15.53993994372673981, 7.305634244248866343E-16 ) ) ;
#2136 = DIRECTION ( 'NONE',  ( 0.000000000000000000, 0.000000000000000000, -1.000000000000000000 ) ) ;
#2137 = VERTEX_POINT ( 'NONE', #12394 ) ;
#2138 = ORIENTED_EDGE ( 'NONE', *, *, #3221, .T. ) ;
#2139 = DIRECTION ( 'NONE',  ( 0.000000000000000000, 0.000000000000000000, -1.000000000000000000 ) ) ;
#2140 = DIRECTION ( 'NONE',  ( -0.000000000000000000, -0.000000000000000000, -1.000000000000000000 ) ) ;
#2141 = CIRCLE ( 'NONE', #3913, 1.700000000000000178 ) ;
#2142 = VERTEX_POINT ( 'NONE', #11291 ) ;
#2143 = DIRECTION ( 'NONE',  ( -1.000000000000000000, 0.000000000000000000, 0.000000000000000000 ) ) ;
#2144 = CARTESIAN_POINT ( 'NONE',  ( 184.0000000000000568, 15.53993994372673626, 47.49999999999997868 ) ) ;
#2145 = CYLINDRICAL_SURFACE ( 'NONE', #8084, 1.499999999999994449 ) ;
#2146 = ORIENTED_EDGE ( 'NONE', *, *, #4376, .F. ) ;
#2147 = VECTOR ( 'NONE', #6810, 1000.000000000000000 ) ;
#2148 = ADVANCED_FACE ( 'NONE', ( #12468 ), #14629, .F. ) ;
#2149 = FILL_AREA_STYLE_COLOUR ( '', #12345 ) ;
#2150 = VERTEX_POINT ( 'NONE', #376 ) ;
#2151 = AXIS2_PLACEMENT_3D ( 'NONE', #14466, #9590, #14388 ) ;
#2152 = LINE ( 'NONE', #1188, #13732 ) ;
#2153 = CARTESIAN_POINT ( 'NONE',  ( -64.00000000000002842, 15.03993994372673981, -2.575184203610571654 ) ) ;
#2154 = FACE_OUTER_BOUND ( 'NONE', #3928, .T. ) ;
#2155 = VERTEX_POINT ( 'NONE', #1811 ) ;
#2156 = CARTESIAN_POINT ( 'NONE',  ( -181.0860728093183809, 120.2032420692993071, -3.023257939496618807 ) ) ;
#2157 = CARTESIAN_POINT ( 'NONE',  ( 194.7298858349713271, 47.80990288192585780, -8.002378029496236778 ) ) ;
#2158 = EDGE_LOOP ( 'NONE', ( #9288, #2472 ) ) ;
#2159 = VECTOR ( 'NONE', #14026, 1000.000000000000114 ) ;
#2160 = CARTESIAN_POINT ( 'NONE',  ( -110.0000000000000426, 19.53993994372674337, 9.999999999999998224 ) ) ;
#2161 = CARTESIAN_POINT ( 'NONE',  ( 0.02311621069196296077, -0.5352285650541119821, -2.750000000000001332 ) ) ;
#2162 = TOROIDAL_SURFACE ( 'NONE', #3174, 1.000000000000000000, 0.5000000000000000000 ) ;
#2163 = EDGE_CURVE ( 'NONE', #7275, #15150, #13731, .T. ) ;
#2164 = DIRECTION ( 'NONE',  ( 0.000000000000000000, 0.000000000000000000, -1.000000000000000000 ) ) ;
#2165 = ORIENTED_EDGE ( 'NONE', *, *, #5654, .T. ) ;
#2166 = DIRECTION ( 'NONE',  ( 1.000000000000000000, 0.000000000000000000, 0.000000000000000000 ) ) ;
#2167 = EDGE_CURVE ( 'NONE', #138, #12060, #13112, .T. ) ;
#2168 = SURFACE_SIDE_STYLE ('',( #10866 ) ) ;
#2169 = EDGE_CURVE ( 'NONE', #8061, #13697, #760, .T. ) ;
#2170 = CARTESIAN_POINT ( 'NONE',  ( 191.4249991583111523, 42.11970308376083949, -6.062475933048471433 ) ) ;
#2171 = VERTEX_POINT ( 'NONE', #12626 ) ;
#2172 = PLANE ( 'NONE',  #4664 ) ;
#2173 = CARTESIAN_POINT ( 'NONE',  ( -214.8265656857867327, 135.2606554265309740, 3.478895870929493483 ) ) ;
#2174 = EDGE_CURVE ( 'NONE', #11026, #379, #5846, .T. ) ;
#2175 = LINE ( 'NONE', #4545, #12545 ) ;
#2176 = EDGE_CURVE ( 'NONE', #4254, #11465, #1524, .T. ) ;
#2177 = CARTESIAN_POINT ( 'NONE',  ( -218.1600191662880661, 152.2676192875508718, 2.431557144026069928 ) ) ;
#2178 = CARTESIAN_POINT ( 'NONE',  ( -76.50000000000001421, 17.53993994372673981, -17.50000000000002487 ) ) ;
#2179 = CIRCLE ( 'NONE', #8249, 1.499999999999994449 ) ;
#2180 = EDGE_LOOP ( 'NONE', ( #5222, #7079 ) ) ;
#2181 = ORIENTED_EDGE ( 'NONE', *, *, #60, .F. ) ;
#2182 = DIRECTION ( 'NONE',  ( 0.000000000000000000, 0.000000000000000000, -1.000000000000000000 ) ) ;
#2183 = CARTESIAN_POINT ( 'NONE',  ( -85.27455057502459113, 65.19100426474074084, -20.00000000000000000 ) ) ;
#2184 = CARTESIAN_POINT ( 'NONE',  ( 0.000000000000000000, 0.000000000000000000, 10.00000000000000178 ) ) ;
#2185 = CARTESIAN_POINT ( 'NONE',  ( 175.9483885134608272, -179.3058001507315566, -17.76585208085566947 ) ) ;
#2186 = CARTESIAN_POINT ( 'NONE',  ( -222.7845331223101084, 143.6298233191951113, -2.509092009812623925 ) ) ;
#2187 = CARTESIAN_POINT ( 'NONE',  ( -223.5258475410019230, 142.2005172455266973, 4.260778343889476183 ) ) ;
#2188 = EDGE_CURVE ( 'NONE', #8586, #1572, #1658, .T. ) ;
#2189 = EDGE_CURVE ( 'NONE', #12185, #15218, #2286, .T. ) ;
#2190 = EDGE_CURVE ( 'NONE', #7996, #6134, #5063, .T. ) ;
#2191 = DIRECTION ( 'NONE',  ( 1.000000000000000000, 0.000000000000000000, 0.000000000000000000 ) ) ;
#2192 = FACE_OUTER_BOUND ( 'NONE', #1666, .T. ) ;
#2193 = CARTESIAN_POINT ( 'NONE',  ( -64.00000000000002842, 14.90076684276668040, -2.084916134869000182 ) ) ;
#2194 = CARTESIAN_POINT ( 'NONE',  ( -76.50000000000001421, 14.97035339324670922, -2.580050169239785696 ) ) ;
#2195 = CARTESIAN_POINT ( 'NONE',  ( 124.2806775638430281, 45.00321902537314145, 10.00000000000000178 ) ) ;
#2196 = CARTESIAN_POINT ( 'NONE',  ( -81.77455057502459113, 65.19100426474074084, 9.975000000000001421 ) ) ;
#2197 = ORIENTED_EDGE ( 'NONE', *, *, #2206, .T. ) ;
#2198 =( NAMED_UNIT ( * ) SI_UNIT ( $, .STERADIAN. ) SOLID_ANGLE_UNIT ( ) );
#2199 = ORIENTED_EDGE ( 'NONE', *, *, #12619, .T. ) ;
#2200 = CARTESIAN_POINT ( 'NONE',  ( -64.00000000000002842, 15.03993994372673804, 38.07518420361041933 ) ) ;
#2201 = CIRCLE ( 'NONE', #13024, 1.700000000000007061 ) ;
#2202 = LINE ( 'NONE', #5913, #10890 ) ;
#2203 = CARTESIAN_POINT ( 'NONE',  ( 64.00000000000005684, 64.51493994372674479, 15.00000000000070166 ) ) ;
#2204 = CARTESIAN_POINT ( 'NONE',  ( -85.99999999999994316, 64.53993994372673626, 15.00000000000174794 ) ) ;
#2205 = CARTESIAN_POINT ( 'NONE',  ( 164.0000000000000568, 56.53993994372675047, 13.29999999999999538 ) ) ;
#2206 = EDGE_CURVE ( 'NONE', #326, #1809, #3, .T. ) ;
#2207 = EDGE_LOOP ( 'NONE', ( #7998, #697, #11706, #6584 ) ) ;
#2208 = ITEM_DEFINED_TRANSFORMATION ( 'NONE', 'NONE', #4491,  #12337 ) ;
#2209 = TOROIDAL_SURFACE ( 'NONE', #683, 1.000000000000000000, 0.5000000000000000000 ) ;
#2210 = VERTEX_POINT ( 'NONE', #1496 ) ;
#2211 = CARTESIAN_POINT ( 'NONE',  ( 203.2625657313046190, 29.78760669494945645, -9.693656633365744568 ) ) ;
#2212 = CARTESIAN_POINT ( 'NONE',  ( 4.030182763035961013E-15, -0.7818963812180698136, 8.000000000000007105 ) ) ;
#2213 = EDGE_LOOP ( 'NONE', ( #2493, #9022, #3912, #7323, #9627 ) ) ;
#2214 = DIRECTION ( 'NONE',  ( 0.000000000000000000, 0.000000000000000000, 1.000000000000000000 ) ) ;
#2215 = FACE_OUTER_BOUND ( 'NONE', #12535, .T. ) ;
#2216 = ORIENTED_EDGE ( 'NONE', *, *, #4024, .T. ) ;
#2217 = VERTEX_POINT ( 'NONE', #8702 ) ;
#2218 = DIRECTION ( 'NONE',  ( -0.000000000000000000, -0.000000000000000000, 1.000000000000000000 ) ) ;
#2219 = DIRECTION ( 'NONE',  ( -1.000000000000000000, -0.000000000000000000, -0.000000000000000000 ) ) ;
#2220 = VERTEX_POINT ( 'NONE', #13494 ) ;
#2221 = AXIS2_PLACEMENT_3D ( 'NONE', #4392, #8047, #15272 ) ;
#2222 = CARTESIAN_POINT ( 'NONE',  ( 164.0000000000000568, 64.53993994372673626, 18.50000000000000711 ) ) ;
#2223 = EDGE_CURVE ( 'NONE', #8472, #9409, #2698, .T. ) ;
#2224 = CIRCLE ( 'NONE', #4232, 1.500000000000001332 ) ;
#2225 = LINE ( 'NONE', #4987, #6382 ) ;
#2226 = EDGE_LOOP ( 'NONE', ( #11645, #7359, #12227, #1854 ) ) ;
#2227 = AXIS2_PLACEMENT_3D ( 'NONE', #510, #15040, #6392 ) ;
#2228 = AXIS2_PLACEMENT_3D ( 'NONE', #6847, #14083, #3283 ) ;
#2229 = CARTESIAN_POINT ( 'NONE',  ( 178.0000000000000853, 15.53993994372673981, -2.500000000000070610 ) ) ;
#2230 = VECTOR ( 'NONE', #255, 1000.000000000000000 ) ;
#2231 = CARTESIAN_POINT ( 'NONE',  ( -167.5010204568278027, 127.4382611495783237, 1.515441478572621570 ) ) ;
#2232 = ADVANCED_FACE ( 'NONE', ( #9967 ), #11147, .F. ) ;
#2233 = DIRECTION ( 'NONE',  ( 0.000000000000000000, 0.000000000000000000, 1.000000000000000000 ) ) ;
#2234 = ORIENTED_EDGE ( 'NONE', *, *, #8634, .F. ) ;
#2235 = CARTESIAN_POINT ( 'NONE',  ( -183.7136537759689929, 127.7093858820786068, -5.230826428279597096 ) ) ;
#2236 = CARTESIAN_POINT ( 'NONE',  ( 193.0816233526163046, 46.15577860858359571, -4.879990690958216248 ) ) ;
#2237 = ORIENTED_EDGE ( 'NONE', *, *, #11806, .T. ) ;
#2238 = EDGE_CURVE ( 'NONE', #6121, #2947, #1017, .T. ) ;
#2239 = CARTESIAN_POINT ( 'NONE',  ( -64.00000000000002842, -178.6666270497714777, -18.18093594598673945 ) ) ;
#2240 = CARTESIAN_POINT ( 'NONE',  ( 0.1709786460663497709, -1.329147683178129924, -2.750000000000000888 ) ) ;
#2241 = CONICAL_SURFACE ( 'NONE', #1478, 2.749999999999999112, 1.047197551196600296 ) ;
#2242 = CARTESIAN_POINT ( 'NONE',  ( -151.9050178466339105, 106.3942781637374679, -4.320071790863974748 ) ) ;
#2243 = VECTOR ( 'NONE', #15562, 1000.000000000000000 ) ;
#2244 = VECTOR ( 'NONE', #232, 1000.000000000000000 ) ;
#2245 = ORIENTED_EDGE ( 'NONE', *, *, #11257, .F. ) ;
#2246 = EDGE_CURVE ( 'NONE', #8808, #9261, #8232, .T. ) ;
#2247 = CARTESIAN_POINT ( 'NONE',  ( 0.7145311798163189732, 4.618802153516981868, -7.999999999999979572 ) ) ;
#2248 = CARTESIAN_POINT ( 'NONE',  ( 207.0703735592109069, 35.50494473061488065, -6.238171316985951620 ) ) ;
#2249 = EDGE_LOOP ( 'NONE', ( #9218, #10170, #8571, #13907 ) ) ;
#2250 = CARTESIAN_POINT ( 'NONE',  ( 190.5000000000000568, -179.8058001507315566, -29.88378295107906624 ) ) ;
#2251 = CARTESIAN_POINT ( 'NONE',  ( -175.7482920159357604, 118.3486081613139334, 7.749957389927518925 ) ) ;
#2252 = AXIS2_PLACEMENT_3D ( 'NONE', #1130, #15560, #8420 ) ;
#2253 = LINE ( 'NONE', #15574, #2995 ) ;
#2254 = CARTESIAN_POINT ( 'NONE',  ( 0.7145311798163258565, 9.237604307034018802, 0.000000000000000000 ) ) ;
#2255 = AXIS2_PLACEMENT_3D ( 'NONE', #7461, #12257, #14467 ) ;
#2256 = CARTESIAN_POINT ( 'NONE',  ( 198.9111841706756536, 32.15857605477618364, -5.308824953579920347 ) ) ;
#2257 = AXIS2_PLACEMENT_3D ( 'NONE', #12770, #9315, #9238 ) ;
#2258 = ORIENTED_EDGE ( 'NONE', *, *, #8099, .F. ) ;
#2259 = ORIENTED_EDGE ( 'NONE', *, *, #13517, .F. ) ;
#2260 = LINE ( 'NONE', #7330, #4538 ) ;
#2261 = CARTESIAN_POINT ( 'NONE',  ( -127.3091761562077409, 106.2673160437096413, 5.000000000000000000 ) ) ;
#2262 = EDGE_CURVE ( 'NONE', #8929, #9928, #5687, .T. ) ;
#2263 = DIRECTION ( 'NONE',  ( 1.000000000000000000, 0.000000000000000000, 0.000000000000000000 ) ) ;
#2264 = CARTESIAN_POINT ( 'NONE',  ( 193.1062858801516882, 40.86394065090267702, 18.00000000000001066 ) ) ;
#2265 = VECTOR ( 'NONE', #3204, 1000.000000000000000 ) ;
#2266 = CARTESIAN_POINT ( 'NONE',  ( -225.1194665507443915, 143.9023506720278647, -1.657832751462523291 ) ) ;
#2267 = AXIS2_PLACEMENT_3D ( 'NONE', #12719, #10820, #8529 ) ;
#2268 = CARTESIAN_POINT ( 'NONE',  ( -222.8945441032406052, 143.4659034320898172, 7.188384078066360594 ) ) ;
#2269 = DIRECTION ( 'NONE',  ( -0.000000000000000000, -0.000000000000000000, 1.000000000000000000 ) ) ;
#2270 = DIRECTION ( 'NONE',  ( 0.000000000000000000, 0.1391731009600660485, -0.9902680687415702510 ) ) ;
#2271 = CARTESIAN_POINT ( 'NONE',  ( -156.3659111473432404, 109.2018789623903814, 9.312033302791148159 ) ) ;
#2272 = CYLINDRICAL_SURFACE ( 'NONE', #431, 0.4999999999999996114 ) ;
#2273 = AXIS2_PLACEMENT_3D ( 'NONE', #7860, #4271, #11240 ) ;
#2274 = DIRECTION ( 'NONE',  ( 1.000000000000000000, 0.000000000000000000, 0.000000000000000000 ) ) ;
#2275 = VERTEX_POINT ( 'NONE', #2205 ) ;
#2276 = AXIS2_PLACEMENT_3D ( 'NONE', #3759, #7408, #3678 ) ;
#2277 = CIRCLE ( 'NONE', #12605, 23.41351791792154202 ) ;
#2278 = EDGE_LOOP ( 'NONE', ( #2374, #13185 ) ) ;
#2279 = CARTESIAN_POINT ( 'NONE',  ( 186.1005832062958234, 72.46888774096882457, 10.00000000000000178 ) ) ;
#2280 = CARTESIAN_POINT ( 'NONE',  ( 202.9928097691983169, 48.86380790798758511, -0.9029304599467440351 ) ) ;
#2281 = ADVANCED_FACE ( 'NONE', ( #7036 ), #14041, .T. ) ;
#2282 = CARTESIAN_POINT ( 'NONE',  ( -185.2055264765504887, 137.3096093875189467, 2.500000000000000000 ) ) ;
#2283 = DIRECTION ( 'NONE',  ( -0.000000000000000000, 0.000000000000000000, -1.000000000000000000 ) ) ;
#2285 = EDGE_CURVE ( 'NONE', #15155, #7716, #15220, .T. ) ;
#2284 = EDGE_CURVE ( 'NONE', #8811, #8894, #6726, .T. ) ;
#2286 = CIRCLE ( 'NONE', #9349, 3.500000000000003109 ) ;
#2287 = B_SPLINE_CURVE_WITH_KNOTS ( 'NONE', 3,
 ( #9719, #2846, #12229, #14514, #206, #5055, #2688, #11138, #13559, #6405, #11214, #6171, #2763, #14745, #13639, #14817, #3943, #3869, #7668, #133, #9880, #1407, #6240, #292, #367, #14590, #8764, #8694, #6092, #3792, #8614, #13411, #5208, #13484, #14670, #2609, #7590, #7507 ),
 .UNSPECIFIED., .F., .F.,
 ( 4, 2, 2, 2, 2, 2, 2, 2, 2, 2, 2, 2, 2, 2, 2, 2, 2, 2, 4 ),
 ( 0.03344994383916276293, 0.03451359215648128198, 0.03557724047379980103, 0.03664088879111832009, 0.03770453710843683914, 0.03876818542575535820, 0.03983183374307387725, 0.04089548206039239631, 0.04195913037771091536, 0.04249095453637018877, 0.04302277869502946217, 0.04408642701234789796, 0.04515007532966634068, 0.04621372364698477647, 0.04727737196430321920, 0.04780919612296243015, 0.04834102028162165499, 0.04940466859894009077, 0.05046831691625852656 ),
 .UNSPECIFIED. ) ;
#2288 = ORIENTED_EDGE ( 'NONE', *, *, #7223, .F. ) ;
#2289 = AXIS2_PLACEMENT_3D ( 'NONE', #6935, #12674, #9375 ) ;
#2290 = ORIENTED_EDGE ( 'NONE', *, *, #3840, .T. ) ;
#2291 = CARTESIAN_POINT ( 'NONE',  ( 205.4699394944333051, 33.88363592193200446, -7.930995773285529182 ) ) ;
#2292 = CARTESIAN_POINT ( 'NONE',  ( 14.00000000000004086, 62.13993994372673768, 16.70000000000105089 ) ) ;
#2293 = VERTEX_POINT ( 'NONE', #3231 ) ;
#2294 = CARTESIAN_POINT ( 'NONE',  ( -35.99999999999995026, 56.53993994372675047, 15.00000000000139977 ) ) ;
#2295 = CARTESIAN_POINT ( 'NONE',  ( -223.0729251748932427, 143.1115555702249083, 6.635881932953087592 ) ) ;
#2296 = VERTEX_POINT ( 'NONE', #8155 ) ;
#2297 = ORIENTED_EDGE ( 'NONE', *, *, #549, .F. ) ;
#2298 = DIRECTION ( 'NONE',  ( 0.000000000000000000, -0.9902680687415713612, 0.1391731009600582492 ) ) ;
#2299 = DIRECTION ( 'NONE',  ( 0.000000000000000000, 1.156482317317871478E-16, -1.000000000000000000 ) ) ;
#2300 = VECTOR ( 'NONE', #3480, 1000.000000000000000 ) ;
#2301 = ORIENTED_EDGE ( 'NONE', *, *, #12956, .F. ) ;
#2302 = CARTESIAN_POINT ( 'NONE',  ( -150.6066609957502180, 106.6619251280432223, 9.538603418629666209 ) ) ;
#2303 = DIRECTION ( 'NONE',  ( -0.4873681696970824651, -0.8731965799097680669, 0.000000000000000000 ) ) ;
#2304 = VECTOR ( 'NONE', #12784, 1000.000000000000000 ) ;
#2305 = DIRECTION ( 'NONE',  ( -0.4999999999999997224, -0.8660254037844387076, 0.000000000000000000 ) ) ;
#2306 = ORIENTED_EDGE ( 'NONE', *, *, #14175, .T. ) ;
#2307 = VECTOR ( 'NONE', #6012, 1000.000000000000000 ) ;
#2308 = ORIENTED_EDGE ( 'NONE', *, *, #12304, .F. ) ;
#2309 = DIRECTION ( 'NONE',  ( 1.000000000000000000, 0.000000000000000000, 0.000000000000000000 ) ) ;
#2310 = AXIS2_PLACEMENT_3D ( 'NONE', #10496, #7027, #1003 ) ;
#2311 = FACE_BOUND ( 'NONE', #3877, .T. ) ;
#2312 = EDGE_LOOP ( 'NONE', ( #1237, #13218, #15094, #2290 ) ) ;
#2313 = CARTESIAN_POINT ( 'NONE',  ( -70.00000000000000000, 15.53993994372673981, -12.49999999999999289 ) ) ;
#2314 = EDGE_CURVE ( 'NONE', #2984, #13426, #3159, .T. ) ;
#2315 = CARTESIAN_POINT ( 'NONE',  ( -211.2987210398670186, 151.8733316563206586, 2.500000000000000000 ) ) ;
#2316 = CARTESIAN_POINT ( 'NONE',  ( 0.7145311798163189732, 4.618802153516981868, -7.999999999999979572 ) ) ;
#2317 = ORIENTED_EDGE ( 'NONE', *, *, #4716, .T. ) ;
#2318 = ORIENTED_EDGE ( 'NONE', *, *, #3155, .F. ) ;
#2319 = CARTESIAN_POINT ( 'NONE',  ( -214.8672114436478466, 153.8753479842104355, 1.515441477536284998 ) ) ;
#2320 = UNCERTAINTY_MEASURE_WITH_UNIT (LENGTH_MEASURE( 1.000000000000000082E-05 ), #15284, 'distance_accuracy_value', 'NONE');
#2321 = CARTESIAN_POINT ( 'NONE',  ( 193.1767286061335653, 35.44822858574072910, -7.249992917093472933 ) ) ;
#2322 = EDGE_LOOP ( 'NONE', ( #9063, #9365, #1627, #14599, #3492, #10575 ) ) ;
#2323 = CIRCLE ( 'NONE', #11152, 1.000000000000000888 ) ;
#2324 = CARTESIAN_POINT ( 'NONE',  ( 5.799999999999999822, 0.000000000000000000, 0.000000000000000000 ) ) ;
#2325 = DIRECTION ( 'NONE',  ( -0.000000000000000000, -0.000000000000000000, -1.000000000000000000 ) ) ;
#2326 = CONICAL_SURFACE ( 'NONE', #13149, 2.749999999999999112, 1.047197551196600296 ) ;
#2327 = CARTESIAN_POINT ( 'NONE',  ( 178.0000000000000853, 15.03993994372673804, 37.57518420361041933 ) ) ;
#2328 = EDGE_LOOP ( 'NONE', ( #14742, #2416, #6007, #15228 ) ) ;
#2329 = DIRECTION ( 'NONE',  ( 0.000000000000000000, -1.000000000000000000, -1.156482317317871725E-16 ) ) ;
#2330 =( NAMED_UNIT ( * ) PLANE_ANGLE_UNIT ( ) SI_UNIT ( $, .RADIAN. ) );
#2331 = EDGE_CURVE ( 'NONE', #4918, #326, #9246, .T. ) ;
#2332 = CARTESIAN_POINT ( 'NONE',  ( 191.3918663844754349, 39.68659111044760124, -5.934329888686073140 ) ) ;
#2333 = ORIENTED_EDGE ( 'NONE', *, *, #2062, .F. ) ;
#2334 = CARTESIAN_POINT ( 'NONE',  ( 205.1062858801516597, 40.86394065090267702, 12.00000000000001066 ) ) ;
#2335 = CARTESIAN_POINT ( 'NONE',  ( 13.91029453487719181, 40.04259805664093363, 9.975000000000001421 ) ) ;
#2336 = CARTESIAN_POINT ( 'NONE',  ( -182.0950013669840359, 118.3955881831737997, 3.410453015226076801 ) ) ;
#2337 = CARTESIAN_POINT ( 'NONE',  ( 5.799999999999999822, -2.775557561562891351E-14, -8.000000000000007105 ) ) ;
#2338 = LINE ( 'NONE', #3444, #2514 ) ;
#2339 = CARTESIAN_POINT ( 'NONE',  ( -170.8670245162619779, 127.1065088405712373, 7.890326795182211583 ) ) ;
#2340 = AXIS2_PLACEMENT_3D ( 'NONE', #4332, #4572, #8066 ) ;
#2341 = CARTESIAN_POINT ( 'NONE',  ( 207.1131222881253393, 35.56952893079440514, -7.807171136772324438 ) ) ;
#2342 = EDGE_LOOP ( 'NONE', ( #3842, #7278 ) ) ;
#2343 = ORIENTED_EDGE ( 'NONE', *, *, #13260, .T. ) ;
#2344 = DIRECTION ( 'NONE',  ( 0.000000000000000000, 1.000000000000000000, 0.000000000000000000 ) ) ;
#2345 = FACE_BOUND ( 'NONE', #12155, .T. ) ;
#2346 = LINE ( 'NONE', #13458, #12195 ) ;
#2347 = PLANE ( 'NONE',  #10254 ) ;
#2348 = CARTESIAN_POINT ( 'NONE',  ( -224.5619895614427435, 144.9011582074930971, 1.476530791908167606 ) ) ;
#2349 = CARTESIAN_POINT ( 'NONE',  ( -219.6010272286711142, 149.7497771715804618, 9.815441629410450730 ) ) ;
#2350 = DIRECTION ( 'NONE',  ( 1.000000000000000000, -0.000000000000000000, -0.000000000000000000 ) ) ;
#2351 = DIRECTION ( 'NONE',  ( 1.000000000000000000, 0.000000000000000000, 0.000000000000000000 ) ) ;
#2352 = EDGE_CURVE ( 'NONE', #1955, #4389, #2032, .T. ) ;
#2353 = CARTESIAN_POINT ( 'NONE',  ( -171.0277344788851792, 115.6541280562350664, 2.431557144026069928 ) ) ;
#2354 = DIRECTION ( 'NONE',  ( -0.000000000000000000, 0.000000000000000000, 1.000000000000000000 ) ) ;
#2355 = VERTEX_POINT ( 'NONE', #10502 ) ;
#2356 = EDGE_LOOP ( 'NONE', ( #9737, #192 ) ) ;
#2357 = CARTESIAN_POINT ( 'NONE',  ( -64.00000000000002842, 15.03993994372673804, 38.07518420361041933 ) ) ;
#2358 = CARTESIAN_POINT ( 'NONE',  ( 114.0000000000000568, 59.53993994372674337, 15.00000000000035172 ) ) ;
#2359 = CIRCLE ( 'NONE', #7167, 1.499999999999994449 ) ;
#2360 = CARTESIAN_POINT ( 'NONE',  ( 184.0000000000000568, -181.3058001507315566, -42.95141194869119516 ) ) ;
#2361 = FILL_AREA_STYLE_COLOUR ( '', #312 ) ;
#2362 = CARTESIAN_POINT ( 'NONE',  ( 0.1097966057365644815, 1.070857859038820248, 2.750000000000000444 ) ) ;
#2363 = DIRECTION ( 'NONE',  ( 0.000000000000000000, -6.938893903907222067E-15, 1.000000000000000000 ) ) ;
#2364 = CARTESIAN_POINT ( 'NONE',  ( -177.3557003870508595, 132.9282874014947140, 2.500000000000000000 ) ) ;
#2365 = VECTOR ( 'NONE', #14176, 1000.000000000000000 ) ;
#2367 = ORIENTED_EDGE ( 'NONE', *, *, #2169, .F. ) ;
#2366 = EDGE_CURVE ( 'NONE', #14692, #10673, #617, .T. ) ;
#2368 = ORIENTED_EDGE ( 'NONE', *, *, #823, .T. ) ;
#2369 = CONICAL_SURFACE ( 'NONE', #11202, 8.000000000000028422, 1.047197551196600296 ) ;
#2370 = CARTESIAN_POINT ( 'NONE',  ( 207.1558710170397433, 35.63411313097393673, -9.376170956558697256 ) ) ;
#2371 = EDGE_CURVE ( 'NONE', #3949, #591, #8596, .T. ) ;
#2372 = EDGE_CURVE ( 'NONE', #12019, #9039, #1775, .T. ) ;
#2373 = CARTESIAN_POINT ( 'NONE',  ( 224.0000000000000853, 56.53993994372675047, 13.00000000000000178 ) ) ;
#2374 = ORIENTED_EDGE ( 'NONE', *, *, #6336, .F. ) ;
#2375 = VECTOR ( 'NONE', #1092, 1000.000000000000000 ) ;
#2376 = CARTESIAN_POINT ( 'NONE',  ( -224.2465401054903964, 145.4663354250427574, 5.241715744539080291 ) ) ;
#2377 = ORIENTED_EDGE ( 'NONE', *, *, #9816, .F. ) ;
#2378 = EDGE_CURVE ( 'NONE', #7650, #12538, #5577, .T. ) ;
#2379 = ORIENTED_EDGE ( 'NONE', *, *, #9833, .F. ) ;
#2380 = LINE ( 'NONE', #9727, #15592 ) ;
#2381 = CARTESIAN_POINT ( 'NONE',  ( 190.5000000000000853, 16.03993994372673626, 37.49999999999991473 ) ) ;
#2382 = ORIENTED_EDGE ( 'NONE', *, *, #8690, .F. ) ;
#2383 = LINE ( 'NONE', #3643, #7585 ) ;
#2384 = VECTOR ( 'NONE', #5148, 1000.000000000000000 ) ;
#2385 = CARTESIAN_POINT ( 'NONE',  ( -76.50000000000001421, 17.53993994372674692, -17.50000000000002487 ) ) ;
#2386 = VERTEX_POINT ( 'NONE', #3316 ) ;
#2387 = EDGE_CURVE ( 'NONE', #7406, #810, #9610, .T. ) ;
#2388 = EDGE_CURVE ( 'NONE', #6288, #10688, #1960, .T. ) ;
#2389 = ORIENTED_EDGE ( 'NONE', *, *, #13377, .F. ) ;
#2390 = CARTESIAN_POINT ( 'NONE',  ( 178.0000000000000853, -179.8058001507315566, -17.19066787724516843 ) ) ;
#2391 = VECTOR ( 'NONE', #14651, 1000.000000000000000 ) ;
#2392 = DIRECTION ( 'NONE',  ( -0.8731965799097685110, 0.4873681696970817434, 0.000000000000000000 ) ) ;
#2393 = LINE ( 'NONE', #2631, #15595 ) ;
#2394 = VERTEX_POINT ( 'NONE', #4574 ) ;
#2395 = ORIENTED_EDGE ( 'NONE', *, *, #5493, .F. ) ;
#2396 = CARTESIAN_POINT ( 'NONE',  ( -187.9088347589046748, 138.8287307560422903, 1.515441477536284109 ) ) ;
#2397 = CARTESIAN_POINT ( 'NONE',  ( 198.3905366428873549, 52.61667164843417765, -5.260075093946414704 ) ) ;
#2398 = ORIENTED_EDGE ( 'NONE', *, *, #14658, .T. ) ;
#2399 = CARTESIAN_POINT ( 'NONE',  ( -76.00000000000001421, 15.03993994372673981, 10.05257423913146475 ) ) ;
#2400 = CARTESIAN_POINT ( 'NONE',  ( -151.4086188282879277, 107.2728346664360259, 84.88378295107887084 ) ) ;
#2401 = FACE_OUTER_BOUND ( 'NONE', #10998, .T. ) ;
#2402 = ADVANCED_FACE ( 'NONE', ( #9396, #5612 ), #4334, .F. ) ;
#2403 = VECTOR ( 'NONE', #11486, 1000.000000000000000 ) ;
#2404 = EDGE_LOOP ( 'NONE', ( #11306, #9340, #9210, #49 ) ) ;
#2405 = CARTESIAN_POINT ( 'NONE',  ( 0.3173508448886365740, 5.375634714784594870, -6.689127551061989863 ) ) ;
#2406 = CARTESIAN_POINT ( 'NONE',  ( 201.3402840685550643, 32.17245832385849980, -2.180909807981465054 ) ) ;
#2407 = VERTEX_POINT ( 'NONE', #11611 ) ;
#2408 = DIRECTION ( 'NONE',  ( 1.000000000000000000, 0.000000000000000000, 0.000000000000000000 ) ) ;
#2409 = DIRECTION ( 'NONE',  ( 1.000000000000000000, 0.000000000000000000, 0.000000000000000000 ) ) ;
#2410 = CARTESIAN_POINT ( 'NONE',  ( -176.4886329031608909, 117.0201139606268441, 5.242686462712208062 ) ) ;
#2411 = DIRECTION ( 'NONE',  ( 0.000000000000000000, 1.156482317317871725E-16, -1.000000000000000000 ) ) ;
#2412 = VERTEX_POINT ( 'NONE', #774 ) ;
#2413 = CARTESIAN_POINT ( 'NONE',  ( -189.9062345257129323, 135.2872556402745374, 9.578254705571842109 ) ) ;
#2414 = DIRECTION ( 'NONE',  ( 0.000000000000000000, -1.000000000000000000, -1.486905836551548832E-16 ) ) ;
#2415 = AXIS2_PLACEMENT_3D ( 'NONE', #9182, #9104, #548 ) ;
#2416 = ORIENTED_EDGE ( 'NONE', *, *, #714, .T. ) ;
#2417 = APPLICATION_CONTEXT ( 'automotive_design' ) ;
#2418 = ORIENTED_EDGE ( 'NONE', *, *, #3717, .T. ) ;
#2419 = CARTESIAN_POINT ( 'NONE',  ( 174.2293059057019775, 61.25683321636181233, 5.000000000000000000 ) ) ;
#2420 = DIRECTION ( 'NONE',  ( 1.000000000000000000, 2.751328491981765035E-32, -3.965082230804130220E-16 ) ) ;
#2421 = CIRCLE ( 'NONE', #7731, 1.000000000000000888 ) ;
#2422 = CARTESIAN_POINT ( 'NONE',  ( 177.5000000000000853, 16.03993994372673981, -2.500000000000071498 ) ) ;
#2423 = CARTESIAN_POINT ( 'NONE',  ( -61.94838851346079167, -179.3058001507315566, 52.76585208085545275 ) ) ;
#2424 = EDGE_CURVE ( 'NONE', #3200, #9186, #5461, .T. ) ;
#2425 = DIRECTION ( 'NONE',  ( 0.000000000000000000, 0.000000000000000000, 1.000000000000000000 ) ) ;
#2426 = CARTESIAN_POINT ( 'NONE',  ( -222.6177564301690950, 144.0132851167816170, 7.888750748740434027 ) ) ;
#2427 = DIRECTION ( 'NONE',  ( -0.000000000000000000, 1.000000000000000000, 0.000000000000000000 ) ) ;
#2428 = CARTESIAN_POINT ( 'NONE',  ( -155.6744015425144312, 109.9339595500499343, 9.657855017614867421 ) ) ;
#2429 = CIRCLE ( 'NONE', #1414, 0.5000000000000004441 ) ;
#2430 = CARTESIAN_POINT ( 'NONE',  ( -206.8718859864436581, 149.4025266312245037, 2.500000000000000000 ) ) ;
#2431 = FACE_OUTER_BOUND ( 'NONE', #10418, .T. ) ;
#2432 = ORIENTED_EDGE ( 'NONE', *, *, #13357, .T. ) ;
#2433 = EDGE_CURVE ( 'NONE', #10355, #6706, #5971, .T. ) ;
#2434 =( NAMED_UNIT ( * ) SI_UNIT ( $, .STERADIAN. ) SOLID_ANGLE_UNIT ( ) );
#2435 = ORIENTED_EDGE ( 'NONE', *, *, #7859, .F. ) ;
#2436 = CARTESIAN_POINT ( 'NONE',  ( -85.99999999999994316, 64.53993994372673626, 11.50000000000174438 ) ) ;
#2437 = CYLINDRICAL_SURFACE ( 'NONE', #10901, 3.500000000000003109 ) ;
#2438 = SURFACE_SIDE_STYLE ('',( #7425 ) ) ;
#2439 = CARTESIAN_POINT ( 'NONE',  ( 0.09566599640799448856, 2.915698366337650338, -0.4498622899576186773 ) ) ;
#2440 = DIRECTION ( 'NONE',  ( 0.8731965799097684000, -0.4873681696970815769, -0.000000000000000000 ) ) ;
#2441 = CYLINDRICAL_SURFACE ( 'NONE', #4016, 1.499999999999999778 ) ;
#2442 = DIRECTION ( 'NONE',  ( -0.000000000000000000, 1.000000000000000000, -0.000000000000000000 ) ) ;
#2443 = EDGE_CURVE ( 'NONE', #5220, #9609, #399, .T. ) ;
#2444 = ORIENTED_EDGE ( 'NONE', *, *, #11456, .F. ) ;
#2445 = ITEM_DEFINED_TRANSFORMATION ( 'NONE', 'NONE', #8048,  #12337 ) ;
#2446 = EDGE_LOOP ( 'NONE', ( #15223, #11561, #11556, #13688 ) ) ;
#2447 = CARTESIAN_POINT ( 'NONE',  ( 205.5291621427655002, 33.93354315402728361, -9.500001906449378808 ) ) ;
#2448 = VERTEX_POINT ( 'NONE', #15525 ) ;
#2449 = CARTESIAN_POINT ( 'NONE',  ( -224.4594852000661831, 145.0848108613691920, 4.280488621519050518 ) ) ;
#2450 = ORIENTED_EDGE ( 'NONE', *, *, #10508, .F. ) ;
#2451 = ORIENTED_EDGE ( 'NONE', *, *, #7116, .T. ) ;
#2452 = FACE_OUTER_BOUND ( 'NONE', #3286, .T. ) ;
#2453 = CARTESIAN_POINT ( 'NONE',  ( 0.000000000000000000, 0.000000000000000000, 0.000000000000000000 ) ) ;
#2454 = VERTEX_POINT ( 'NONE', #6084 ) ;
#2455 = DIRECTION ( 'NONE',  ( -0.000000000000000000, -1.000000000000000000, -0.000000000000000000 ) ) ;
#2456 = CARTESIAN_POINT ( 'NONE',  ( -35.99999999999995026, 59.53993994372674337, 15.00000000000139977 ) ) ;
#2457 = EDGE_CURVE ( 'NONE', #9826, #13697, #3699, .T. ) ;
#2458 = DIRECTION ( 'NONE',  ( 1.000000000000000000, 0.000000000000000000, 0.000000000000000000 ) ) ;
#2459 = ORIENTED_EDGE ( 'NONE', *, *, #12208, .T. ) ;
#2460 = CARTESIAN_POINT ( 'NONE',  ( 164.0000000000000568, 64.53993994372673626, 18.52500000000000213 ) ) ;
#2461 = FACE_OUTER_BOUND ( 'NONE', #10931, .T. ) ;
#2462 = ORIENTED_EDGE ( 'NONE', *, *, #12399, .F. ) ;
#2463 = DIRECTION ( 'NONE',  ( 0.000000000000000000, 0.9902680687415713612, -0.1391731009600582492 ) ) ;
#2464 = CIRCLE ( 'NONE', #10537, 1.500000000000001332 ) ;
#2465 = CARTESIAN_POINT ( 'NONE',  ( -174.7846310273254176, 131.4932641812416421, 2.500000000270498735 ) ) ;
#2466 = DIRECTION ( 'NONE',  ( 0.000000000000000000, 0.000000000000000000, 1.000000000000000000 ) ) ;
#2467 = EDGE_LOOP ( 'NONE', ( #14037, #4593 ) ) ;
#2468 = ORIENTED_EDGE ( 'NONE', *, *, #6146, .F. ) ;
#2469 = CARTESIAN_POINT ( 'NONE',  ( -204.1471980322648960, 142.4963817258166614, -4.640918829492428621 ) ) ;
#2470 = CARTESIAN_POINT ( 'NONE',  ( 205.4911088677281725, 33.92184391926740972, -3.501858402168778639 ) ) ;
#2471 = AXIS2_PLACEMENT_3D ( 'NONE', #1350, #8631, #13427 ) ;
#2472 = ORIENTED_EDGE ( 'NONE', *, *, #12766, .F. ) ;
#2473 = ADVANCED_FACE ( 'NONE', ( #10661 ), #14580, .F. ) ;
#2474 = DIRECTION ( 'NONE',  ( 1.000000000000000000, 0.000000000000000000, -0.000000000000000000 ) ) ;
#2475 = DIRECTION ( 'NONE',  ( -1.000000000000000000, 0.000000000000000000, 0.000000000000000000 ) ) ;
#2476 = ADVANCED_FACE ( 'NONE', ( #3546, #1093 ), #1246, .F. ) ;
#2477 = ADVANCED_FACE ( 'NONE', ( #10974, #11918 ), #8528, .F. ) ;
#2478 = CARTESIAN_POINT ( 'NONE',  ( 51.07686401294030532, 368.7106150007013525, 0.000000000000000000 ) ) ;
#2479 = VECTOR ( 'NONE', #14694, 1000.000000000000000 ) ;
#2480 = VERTEX_POINT ( 'NONE', #7200 ) ;
#2481 = VECTOR ( 'NONE', #2055, 1000.000000000000000 ) ;
#2482 = AXIS2_PLACEMENT_3D ( 'NONE', #12280, #12364, #11576 ) ;
#2483 = DIRECTION ( 'NONE',  ( 0.000000000000000000, 0.000000000000000000, 1.000000000000000000 ) ) ;
#2484 = CARTESIAN_POINT ( 'NONE',  ( 198.4239224672526234, 29.08807987246144933, -3.746314016867685837 ) ) ;
#2485 = EDGE_LOOP ( 'NONE', ( #149, #2081 ) ) ;
#2486 = LINE ( 'NONE', #8430, #3319 ) ;
#2487 = FACE_BOUND ( 'NONE', #4495, .T. ) ;
#2488 = CARTESIAN_POINT ( 'NONE',  ( -205.7712766299887335, 131.5939592662764994, -0.4555467707853333992 ) ) ;
#2489 = DIRECTION ( 'NONE',  ( -0.1562424607007877608, 0.2866315678550999668, -0.9452145987991775744 ) ) ;
#2490 = VERTEX_POINT ( 'NONE', #55 ) ;
#2491 = CARTESIAN_POINT ( 'NONE',  ( -173.3366878899875019, 128.3846004176512849, 7.899914667150486736 ) ) ;
#2492 = CARTESIAN_POINT ( 'NONE',  ( 0.000000000000000000, 19.53993994372674337, 2.905405074819403421E-15 ) ) ;
#2493 = ORIENTED_EDGE ( 'NONE', *, *, #12725, .T. ) ;
#2494 = ORIENTED_EDGE ( 'NONE', *, *, #1795, .T. ) ;
#2495 = CIRCLE ( 'NONE', #3505, 3.500000000000003109 ) ;
#2496 = DIRECTION ( 'NONE',  ( -0.7071067811865425767, 8.659560562354994488E-17, -0.7071067811865525687 ) ) ;
#2497 = DIRECTION ( 'NONE',  ( -0.000000000000000000, -0.000000000000000000, 1.000000000000000000 ) ) ;
#2498 = CIRCLE ( 'NONE', #6547, 9.999999999999994671 ) ;
#2499 = CARTESIAN_POINT ( 'NONE',  ( 170.8293059057019718, 61.25683321636181233, 0.000000000000000000 ) ) ;
#2500 = CARTESIAN_POINT ( 'NONE',  ( -63.50000000000002842, 17.53993994372673271, 52.49999999999997868 ) ) ;
#2501 = CARTESIAN_POINT ( 'NONE',  ( -223.5232359142329699, 142.1851836626728129, 0.6707363232510722417 ) ) ;
#2502 = CIRCLE ( 'NONE', #13082, 8.000000000000028422 ) ;
#2503 = CYLINDRICAL_SURFACE ( 'NONE', #320, 1.700000000000000178 ) ;
#2504 = DIRECTION ( 'NONE',  ( 0.000000000000000000, -0.9902680687415714722, 0.1391731009600582769 ) ) ;
#2505 = AXIS2_PLACEMENT_3D ( 'NONE', #4185, #11387, #5471 ) ;
#2506 = CARTESIAN_POINT ( 'NONE',  ( 13.91029453487719181, 40.04259805664093363, 10.00000000000000178 ) ) ;
#2507 = EDGE_CURVE ( 'NONE', #11511, #6265, #10735, .T. ) ;
#2508 = DIRECTION ( 'NONE',  ( 0.000000000000000000, 0.000000000000000000, 1.000000000000000000 ) ) ;
#2509 = FACE_OUTER_BOUND ( 'NONE', #7164, .T. ) ;
#2510 = EDGE_LOOP ( 'NONE', ( #14634, #5325, #7397, #7546 ) ) ;
#2511 = DIRECTION ( 'NONE',  ( 0.000000000000000000, 0.000000000000000000, 1.000000000000000000 ) ) ;
#2512 = ADVANCED_FACE ( 'NONE', ( #13319, #1167, #1325, #5997, #3781, #4967, #10818 ), #15607, .F. ) ;
#2513 = EDGE_LOOP ( 'NONE', ( #6791, #745, #3131, #3579, #74, #985, #2095, #13502, #11369 ) ) ;
#2514 = VECTOR ( 'NONE', #9523, 1000.000000000000000 ) ;
#2515 = CARTESIAN_POINT ( 'NONE',  ( -33.09899788034579871, 48.72489408690345414, 5.000000000000000000 ) ) ;
#2516 = DIRECTION ( 'NONE',  ( 0.000000000000000000, -1.734723475976808672E-15, -1.000000000000000000 ) ) ;
#2517 = VECTOR ( 'NONE', #6749, 1000.000000000000000 ) ;
#2518 = DIRECTION ( 'NONE',  ( 3.965082230804130220E-16, 1.090924371466202084E-47, 1.000000000000000000 ) ) ;
#2519 = CIRCLE ( 'NONE', #9844, 1.700000000000000178 ) ;
#2520 = CARTESIAN_POINT ( 'NONE',  ( 0.2456200930618618050, 1.587713240271470427, 2.750000000000000888 ) ) ;
#2521 = VECTOR ( 'NONE', #8962, 1000.000000000000000 ) ;
#2522 = CARTESIAN_POINT ( 'NONE',  ( -108.0000000000000568, 64.53993994372673626, 10.00000000000000178 ) ) ;
#2523 = CARTESIAN_POINT ( 'NONE',  ( -198.5721217036497990, 144.7598446228703324, 3.478855109513426580 ) ) ;
#2524 = ORIENTED_EDGE ( 'NONE', *, *, #1604, .F. ) ;
#2525 = AXIS2_PLACEMENT_3D ( 'NONE', #10287, #638, #6595 ) ;
#2526 = AXIS2_PLACEMENT_3D ( 'NONE', #12047, #3605, #9766 ) ;
#2527 = EDGE_LOOP ( 'NONE', ( #2811, #5685, #13665, #9298 ) ) ;
#2528 = CARTESIAN_POINT ( 'NONE',  ( 202.4595012533446550, 32.68412682837883665, -9.685340726858029825 ) ) ;
#2529 = EDGE_CURVE ( 'NONE', #3509, #4053, #4812, .T. ) ;
#2530 = CARTESIAN_POINT ( 'NONE',  ( 190.0000000000000568, -179.3058001507315566, -17.19066787724516843 ) ) ;
#2531 = ORIENTED_EDGE ( 'NONE', *, *, #8498, .T. ) ;
#2532 = CARTESIAN_POINT ( 'NONE',  ( -222.5506325035290729, 148.5048201065549733, 9.875490118357738822 ) ) ;
#2533 = VERTEX_POINT ( 'NONE', #9632 ) ;
#2534 = DIRECTION ( 'NONE',  ( 0.000000000000000000, 0.000000000000000000, 1.000000000000000000 ) ) ;
#2535 = CARTESIAN_POINT ( 'NONE',  ( 209.5863484626195543, 33.70058422559537092, -1.816147585399736863 ) ) ;
#2536 = ORIENTED_EDGE ( 'NONE', *, *, #2882, .F. ) ;
#2537 = DIRECTION ( 'NONE',  ( 0.000000000000000000, -0.1391731009600591096, 0.9902680687415711391 ) ) ;
#2538 = DIRECTION ( 'NONE',  ( -1.000000000000000000, 0.000000000000000000, 0.000000000000000000 ) ) ;
#2539 = CIRCLE ( 'NONE', #5064, 0.5000000000000004441 ) ;
#2540 = EDGE_CURVE ( 'NONE', #15212, #5473, #4448, .T. ) ;
#2541 = AXIS2_PLACEMENT_3D ( 'NONE', #4583, #12869, #12947 ) ;
#2542 = AXIS2_PLACEMENT_3D ( 'NONE', #5724, #10700, #12740 ) ;
#2543 = DIRECTION ( 'NONE',  ( 0.000000000000000000, 1.000000000000000000, 0.000000000000000000 ) ) ;
#2544 = ORIENTED_EDGE ( 'NONE', *, *, #3841, .T. ) ;
#2545 = EDGE_CURVE ( 'NONE', #858, #12940, #3625, .T. ) ;
#2546 = ORIENTED_EDGE ( 'NONE', *, *, #12587, .F. ) ;
#2547 = DIRECTION ( 'NONE',  ( -0.000000000000000000, -0.000000000000000000, 1.000000000000000000 ) ) ;
#2548 = CIRCLE ( 'NONE', #11377, 1.700000000000007061 ) ;
#2549 = CARTESIAN_POINT ( 'NONE',  ( 190.5000000000000853, 14.90076684276667507, 37.08491613486882699 ) ) ;
#2550 = ORIENTED_EDGE ( 'NONE', *, *, #4683, .T. ) ;
#2551 = DIRECTION ( 'NONE',  ( 0.000000000000000000, -1.000000000000000000, 0.000000000000000000 ) ) ;
#2552 = CIRCLE ( 'NONE', #3062, 3.299128011492291623 ) ;
#2553 = EDGE_CURVE ( 'NONE', #299, #9986, #9713, .T. ) ;
#2554 = DIRECTION ( 'NONE',  ( 0.000000000000000000, 0.000000000000000000, -1.000000000000000000 ) ) ;
#2555 = ORIENTED_EDGE ( 'NONE', *, *, #2553, .T. ) ;
#2556 = ORIENTED_EDGE ( 'NONE', *, *, #3184, .F. ) ;
#2557 = CARTESIAN_POINT ( 'NONE',  ( -174.4670243326416994, 126.3579851466298010, -4.682492215613329734 ) ) ;
#2558 = CARTESIAN_POINT ( 'NONE',  ( -36.49899788034579728, 48.72489408690345414, 7.600000000000002309 ) ) ;
#2559 = ORIENTED_EDGE ( 'NONE', *, *, #8634, .T. ) ;
#2560 = CARTESIAN_POINT ( 'NONE',  ( 0.000000000000000000, 0.000000000000000000, 5.000000000000017764 ) ) ;
#2561 = DIRECTION ( 'NONE',  ( -0.000000000000000000, -0.000000000000000000, 1.000000000000000000 ) ) ;
#2562 = CARTESIAN_POINT ( 'NONE',  ( 17.41029453487719181, 40.04259805664093363, 10.00000000000000178 ) ) ;
#2563 = VECTOR ( 'NONE', #14577, 999.9999999999998863 ) ;
#2564 = ORIENTED_EDGE ( 'NONE', *, *, #6517, .F. ) ;
#2565 = ADVANCED_FACE ( 'NONE', ( #14272 ), #3467, .F. ) ;
#2566 = CARTESIAN_POINT ( 'NONE',  ( 190.7088546992480076, 48.18597428004899541, -1.751405883087224113 ) ) ;
#2567 = ORIENTED_EDGE ( 'NONE', *, *, #6390, .F. ) ;
#2568 = CARTESIAN_POINT ( 'NONE',  ( 51.39999999999999858, 0.000000000000000000, 0.000000000000000000 ) ) ;
#2569 = CARTESIAN_POINT ( 'NONE',  ( -221.1246142512582082, 146.8432591943234797, -4.818913680500031660 ) ) ;
#2570 = CARTESIAN_POINT ( 'NONE',  ( -175.7369819406991382, 118.3688719364822646, -3.133266157129962259 ) ) ;
#2573 = EDGE_CURVE ( 'NONE', #14639, #15035, #2678, .T. ) ;
#2572 = EDGE_CURVE ( 'NONE', #2702, #6505, #12293, .T. ) ;
#2571 = DIRECTION ( 'NONE',  ( 0.000000000000000000, 1.000000000000000000, 6.938893903907227145E-17 ) ) ;
#2574 = ADVANCED_FACE ( 'NONE', ( #12221 ), #357, .F. ) ;
#2575 = ORIENTED_EDGE ( 'NONE', *, *, #2352, .T. ) ;
#2576 = CARTESIAN_POINT ( 'NONE',  ( -213.7333075327791789, 137.2030432634720967, 7.918248976830621011 ) ) ;
#2578 = CARTESIAN_POINT ( 'NONE',  ( -173.6473242186147274, 117.1162325653264418, 2.431557144026069928 ) ) ;
#2577 = AXIS2_PLACEMENT_3D ( 'NONE', #13721, #5363, #13638 ) ;
#2579 = ORIENTED_EDGE ( 'NONE', *, *, #10572, .T. ) ;
#2580 = EDGE_LOOP ( 'NONE', ( #5296, #14213, #11579, #14953 ) ) ;
#2581 = EDGE_CURVE ( 'NONE', #6993, #3478, #919, .T. ) ;
#2582 = AXIS2_PLACEMENT_3D ( 'NONE', #10909, #3708, #8537 ) ;
#2583 = LINE ( 'NONE', #5895, #10351 ) ;
#2584 = DIRECTION ( 'NONE',  ( 0.000000000000000000, 0.000000000000000000, -1.000000000000000000 ) ) ;
#2585 = CARTESIAN_POINT ( 'NONE',  ( -70.00000000000000000, 15.53993994372673626, 48.99999999999997158 ) ) ;
#2586 = DIRECTION ( 'NONE',  ( 0.000000000000000000, 0.000000000000000000, -1.000000000000000000 ) ) ;
#2587 = VECTOR ( 'NONE', #6441, 1000.000000000000000 ) ;
#2588 = DIRECTION ( 'NONE',  ( -0.000000000000000000, 1.000000000000000000, -0.000000000000000000 ) ) ;
#2589 = VECTOR ( 'NONE', #4836, 1000.000000000000000 ) ;
#2590 = CARTESIAN_POINT ( 'NONE',  ( -157.1465583139810178, 109.3199373332567603, 9.183240261263447834 ) ) ;
#2591 = EDGE_CURVE ( 'NONE', #6470, #4243, #5199, .T. ) ;
#2592 = DIRECTION ( 'NONE',  ( -0.000000000000000000, 1.000000000000000000, -0.000000000000000000 ) ) ;
#2593 = CYLINDRICAL_SURFACE ( 'NONE', #289, 335.5619230110239641 ) ;
#2594 = ORIENTED_EDGE ( 'NONE', *, *, #3965, .T. ) ;
#2595 = CARTESIAN_POINT ( 'NONE',  ( -3.869242359956847046E-15, -2.652070323102386329, 0.9064794551410519929 ) ) ;
#2596 = ORIENTED_EDGE ( 'NONE', *, *, #137, .F. ) ;
#2597 = DIRECTION ( 'NONE',  ( -0.8731965799097685110, 0.4873681696970816324, -0.000000000000000000 ) ) ;
#2598 = CARTESIAN_POINT ( 'NONE',  ( -168.8345777152483151, 119.5835126658289909, 2.431557144026069928 ) ) ;
#2599 = FILL_AREA_STYLE_COLOUR ( '', #6383 ) ;
#2600 = DIRECTION ( 'NONE',  ( 0.000000000000000000, 0.000000000000000000, -1.000000000000000000 ) ) ;
#2601 = CIRCLE ( 'NONE', #13674, 1.699999999999994849 ) ;
#2602 = DIRECTION ( 'NONE',  ( 0.000000000000000000, 0.000000000000000000, 1.000000000000000000 ) ) ;
#2603 = DIRECTION ( 'NONE',  ( -1.000000000000000000, 0.000000000000000000, 0.000000000000000000 ) ) ;
#2604 = ORIENTED_EDGE ( 'NONE', *, *, #8057, .T. ) ;
#2605 = VECTOR ( 'NONE', #3466, 1000.000000000000000 ) ;
#2606 = EDGE_CURVE ( 'NONE', #7302, #13797, #1412, .T. ) ;
#2607 = DIRECTION ( 'NONE',  ( -0.000000000000000000, -0.000000000000000000, 1.000000000000000000 ) ) ;
#2608 = CARTESIAN_POINT ( 'NONE',  ( 202.3883256910358739, 32.65987148549056229, -8.116337980372584582 ) ) ;
#2609 = CARTESIAN_POINT ( 'NONE',  ( -219.4906341098210589, 153.9872875675930857, 3.763523804975331011 ) ) ;
#2610 = EDGE_LOOP ( 'NONE', ( #6247, #8856 ) ) ;
#2611 = AXIS2_PLACEMENT_3D ( 'NONE', #7905, #841, #9307 ) ;
#2612 = CARTESIAN_POINT ( 'NONE',  ( -223.5303683316520562, 142.1912745150580122, 4.217707172678373695 ) ) ;
#2613 = EDGE_LOOP ( 'NONE', ( #2450, #9720, #11799, #2764 ) ) ;
#2614 = DIRECTION ( 'NONE',  ( -0.000000000000000000, 1.000000000000000000, 1.156482317317871725E-16 ) ) ;
#2615 = LINE ( 'NONE', #7439, #2045 ) ;
#2617 = VERTEX_POINT ( 'NONE', #6553 ) ;
#2616 =( GEOMETRIC_REPRESENTATION_CONTEXT ( 3 ) GLOBAL_UNCERTAINTY_ASSIGNED_CONTEXT ( ( #4060 ) ) GLOBAL_UNIT_ASSIGNED_CONTEXT ( ( #12452, #13713, #2835 ) ) REPRESENTATION_CONTEXT ( 'NONE', 'WORKASPACE' ) );
#2618 = CARTESIAN_POINT ( 'NONE',  ( -150.5341340129182583, 106.7708477820315665, 9.581378567423383785 ) ) ;
#2619 = DIRECTION ( 'NONE',  ( -0.000000000000000000, -0.000000000000000000, 1.000000000000000000 ) ) ;
#2620 = LINE ( 'NONE', #12470, #1574 ) ;
#2621 = EDGE_LOOP ( 'NONE', ( #1993, #8913 ) ) ;
#2622 = CIRCLE ( 'NONE', #12941, 0.4000000000000001887 ) ;
#2623 = EDGE_CURVE ( 'NONE', #6805, #5504, #3445, .T. ) ;
#2624 = DIRECTION ( 'NONE',  ( 1.156482317317871725E-16, -1.156482317317871725E-16, 1.000000000000000000 ) ) ;
#2625 = ORIENTED_EDGE ( 'NONE', *, *, #10969, .T. ) ;
#2626 = CIRCLE ( 'NONE', #9687, 1.500000000000001332 ) ;
#2627 = LINE ( 'NONE', #7376, #597 ) ;
#2628 = CARTESIAN_POINT ( 'NONE',  ( -76.50000000000001421, -178.9449732516916072, -29.32815825124561471 ) ) ;
#2629 = ORIENTED_EDGE ( 'NONE', *, *, #2176, .T. ) ;
#2630 = DIRECTION ( 'NONE',  ( -0.000000000000000000, 0.000000000000000000, 1.000000000000000000 ) ) ;
#2631 = CARTESIAN_POINT ( 'NONE',  ( 190.5000000000000568, 15.10952649420676686, 25.44255979523916977 ) ) ;
#2632 = ORIENTED_EDGE ( 'NONE', *, *, #8001, .T. ) ;
#2633 = ORIENTED_EDGE ( 'NONE', *, *, #15205, .F. ) ;
#2634 = CARTESIAN_POINT ( 'NONE',  ( -212.2154691228631691, 150.1790628786027355, -2.963320117457098224 ) ) ;
#2635 = CARTESIAN_POINT ( 'NONE',  ( 194.7691866843436799, 33.87697957786221536, -2.559886773443665220 ) ) ;
#2636 = ORIENTED_EDGE ( 'NONE', *, *, #10806, .F. ) ;
#2637 = VECTOR ( 'NONE', #300, 1000.000000000000000 ) ;
#2638 = CARTESIAN_POINT ( 'NONE',  ( -85.99999999999994316, 64.53993994372673626, 15.00000000000174794 ) ) ;
#2639 = CARTESIAN_POINT ( 'NONE',  ( -108.0000000000000568, 59.53993994372674337, 10.00000000000000178 ) ) ;
#2640 = DIRECTION ( 'NONE',  ( 0.000000000000000000, 0.000000000000000000, 1.000000000000000000 ) ) ;
#2641 = ADVANCED_FACE ( 'NONE', ( #5123, #10175 ), #7740, .T. ) ;
#2642 = EDGE_CURVE ( 'NONE', #2137, #5720, #8838, .T. ) ;
#2643 = AXIS2_PLACEMENT_3D ( 'NONE', #9058, #10474, #5423 ) ;
#2644 = FACE_BOUND ( 'NONE', #4039, .T. ) ;
#2645 = CARTESIAN_POINT ( 'NONE',  ( 198.5110307061451067, 52.63772278181842523, -5.120705508804510586 ) ) ;
#2646 = ORIENTED_EDGE ( 'NONE', *, *, #1028, .T. ) ;
#2647 = CARTESIAN_POINT ( 'NONE',  ( -64.00000000000002842, -179.8058001507315566, -17.19066787724516843 ) ) ;
#2648 = CARTESIAN_POINT ( 'NONE',  ( -219.5968554534879331, 149.7166363036416215, -4.923873429609202823 ) ) ;
#2649 = CARTESIAN_POINT ( 'NONE',  ( -197.4248861630254055, 135.1594620591177431, -5.230826428279599760 ) ) ;
#2650 = CARTESIAN_POINT ( 'NONE',  ( 177.5000000000000853, 17.53993994372673271, 52.49999999999997868 ) ) ;
#2651 = ORIENTED_EDGE ( 'NONE', *, *, #4189, .T. ) ;
#2652 = CARTESIAN_POINT ( 'NONE',  ( -224.7572118800429735, 144.5513867789856022, 7.859965607560822853 ) ) ;
#2653 = CARTESIAN_POINT ( 'NONE',  ( 203.1375244286944906, 48.81137831324044640, 0.6531691591918254991 ) ) ;
#2654 = VERTEX_POINT ( 'NONE', #12524 ) ;
#2655 = ORIENTED_EDGE ( 'NONE', *, *, #1415, .F. ) ;
#2656 = EDGE_CURVE ( 'NONE', #1137, #235, #6474, .T. ) ;
#2657 = VECTOR ( 'NONE', #5887, 1000.000000000000000 ) ;
#2658 = DIRECTION ( 'NONE',  ( 1.000000000000000000, 0.000000000000000000, 0.000000000000000000 ) ) ;
#2659 = DIRECTION ( 'NONE',  ( 1.000000000000000000, 0.000000000000000000, 0.000000000000000000 ) ) ;
#2660 = CARTESIAN_POINT ( 'NONE',  ( 190.5000000000000853, 15.53993994372673626, 52.49999999999997868 ) ) ;
#2661 = EDGE_CURVE ( 'NONE', #10578, #8016, #14281, .T. ) ;
#2662 = DIRECTION ( 'NONE',  ( 0.000000000000000000, 0.000000000000000000, -1.000000000000000000 ) ) ;
#2663 = EDGE_CURVE ( 'NONE', #2049, #7175, #10775, .T. ) ;
#2664 = EDGE_CURVE ( 'NONE', #6169, #1426, #14784, .T. ) ;
#2665 = DIRECTION ( 'NONE',  ( 0.000000000000000000, 0.000000000000000000, 1.000000000000000000 ) ) ;
#2666 = AXIS2_PLACEMENT_3D ( 'NONE', #12786, #5543, #3098 ) ;
#2667 = CARTESIAN_POINT ( 'NONE',  ( -206.2408270422487249, 148.5277750773568926, 5.434754235172608361 ) ) ;
#2668 = DIRECTION ( 'NONE',  ( 1.000000000000000000, -2.751328491981765035E-32, 3.965082230804130220E-16 ) ) ;
#2669 = DIRECTION ( 'NONE',  ( -0.000000000000000000, 1.000000000000000000, -0.000000000000000000 ) ) ;
#2670 = ORIENTED_EDGE ( 'NONE', *, *, #6962, .F. ) ;
#2671 = AXIS2_PLACEMENT_3D ( 'NONE', #13362, #2561, #2715 ) ;
#2672 = CYLINDRICAL_SURFACE ( 'NONE', #9111, 0.5000000000000004441 ) ;
#2673 = VERTEX_POINT ( 'NONE', #11277 ) ;
#2674 = CARTESIAN_POINT ( 'NONE',  ( 172.5293059057019889, 61.25683321636181233, 9.975000000000001421 ) ) ;
#2675 = LINE ( 'NONE', #14661, #2563 ) ;
#2676 = CARTESIAN_POINT ( 'NONE',  ( 68.56535645333921991, 38.79159067395544014, 5.000000000000000000 ) ) ;
#2677 = CARTESIAN_POINT ( 'NONE',  ( 190.5000000000000568, 15.53993994372673804, 38.07518420361041933 ) ) ;
#2678 = LINE ( 'NONE', #2836, #14526 ) ;
#2679 = CARTESIAN_POINT ( 'NONE',  ( -76.00000000000007105, -179.3058001507315566, 84.88378295107887084 ) ) ;
#2680 = CARTESIAN_POINT ( 'NONE',  ( -207.1387806695930749, 146.9236570583465209, 7.919662025281895446 ) ) ;
#2681 = AXIS2_PLACEMENT_3D ( 'NONE', #673, #11677, #3216 ) ;
#2682 = EDGE_CURVE ( 'NONE', #11943, #3320, #515, .T. ) ;
#2683 = EDGE_CURVE ( 'NONE', #10665, #2814, #929, .T. ) ;
#2684 = EDGE_CURVE ( 'NONE', #8499, #4070, #159, .T. ) ;
#2685 = ORIENTED_EDGE ( 'NONE', *, *, #6294, .T. ) ;
#2686 = DIRECTION ( 'NONE',  ( 1.000000000000000000, -2.751328491981765035E-32, 3.965082230804130220E-16 ) ) ;
#2687 = CARTESIAN_POINT ( 'NONE',  ( -76.50000000000004263, -178.8058001507315566, 65.31842631998698323 ) ) ;
#2688 = CARTESIAN_POINT ( 'NONE',  ( -224.3981447419311905, 145.1947119209457355, 4.619413130059836448 ) ) ;
#2689 = VERTEX_POINT ( 'NONE', #7427 ) ;
#2690 = CARTESIAN_POINT ( 'NONE',  ( -217.0312179575220171, 154.3153628681492364, 5.590069521792075058 ) ) ;
#2691 = ORIENTED_EDGE ( 'NONE', *, *, #11732, .F. ) ;
#2692 = CARTESIAN_POINT ( 'NONE',  ( -173.2167472191050592, 117.8876788491354546, -3.302252044790073615 ) ) ;
#2693 = CARTESIAN_POINT ( 'NONE',  ( -110.0000000000000426, 22.53993994372673981, 13.00000000000000178 ) ) ;
#2694 = EDGE_CURVE ( 'NONE', #3938, #8914, #2201, .T. ) ;
#2695 = AXIS2_PLACEMENT_3D ( 'NONE', #7638, #1622, #11110 ) ;
#2696 = ORIENTED_EDGE ( 'NONE', *, *, #12610, .T. ) ;
#2697 = CARTESIAN_POINT ( 'NONE',  ( -152.4086188282879277, 107.2728346664360259, 0.000000000000000000 ) ) ;
#2698 = LINE ( 'NONE', #7517, #5304 ) ;
#2699 = FACE_BOUND ( 'NONE', #6003, .T. ) ;
#2700 = ORIENTED_EDGE ( 'NONE', *, *, #12306, .T. ) ;
#2701 = DIRECTION ( 'NONE',  ( 0.000000000000000000, -1.000000000000000000, -1.156482317317871725E-16 ) ) ;
#2702 = VERTEX_POINT ( 'NONE', #5045 ) ;
#2703 = CARTESIAN_POINT ( 'NONE',  ( -110.0000000000000426, 19.53993994372674337, 9.999999999999998224 ) ) ;
#2704 = CARTESIAN_POINT ( 'NONE',  ( 126.1056775638430310, 45.00321902537314145, 10.00000000000000178 ) ) ;
#2705 = ORIENTED_EDGE ( 'NONE', *, *, #13825, .T. ) ;
#2706 = CARTESIAN_POINT ( 'NONE',  ( 21.99999999999999289, 1.665213485140613626E-16, -1.219500000000000028 ) ) ;
#2707 = ADVANCED_FACE ( 'NONE', ( #9304 ), #14024, .T. ) ;
#2708 = CARTESIAN_POINT ( 'NONE',  ( 119.0806775638430253, 45.00321902537314145, 7.600000000000002309 ) ) ;
#2709 = ORIENTED_EDGE ( 'NONE', *, *, #3577, .F. ) ;
#2710 = EDGE_LOOP ( 'NONE', ( #11694, #3134, #10364, #520 ) ) ;
#2711 = DIRECTION ( 'NONE',  ( 1.000000000000000000, 0.000000000000000000, 0.000000000000000000 ) ) ;
#2712 = CARTESIAN_POINT ( 'NONE',  ( 208.8124460758720033, 42.05191026284237665, -4.433604294307299298 ) ) ;
#2713 = EDGE_LOOP ( 'NONE', ( #4387, #13395, #7759, #13178, #10615 ) ) ;
#2714 = DIRECTION ( 'NONE',  ( -0.000000000000000000, 1.000000000000000000, -0.000000000000000000 ) ) ;
#2715 = DIRECTION ( 'NONE',  ( 1.000000000000000000, 0.000000000000000000, 0.000000000000000000 ) ) ;
#2716 = LINE ( 'NONE', #5086, #1760 ) ;
#2717 = CIRCLE ( 'NONE', #9538, 1.499999999999997780 ) ;
#2718 = LINE ( 'NONE', #4934, #2587 ) ;
#2719 = EDGE_CURVE ( 'NONE', #591, #3949, #6727, .T. ) ;
#2720 = CARTESIAN_POINT ( 'NONE',  ( 193.1683668805158334, 46.28448754599228465, -1.741988976065122152 ) ) ;
#2721 = ORIENTED_EDGE ( 'NONE', *, *, #9924, .T. ) ;
#2722 = CARTESIAN_POINT ( 'NONE',  ( -64.00000000000002842, -178.7362136002515172, -17.68580191161595394 ) ) ;
#2723 = CARTESIAN_POINT ( 'NONE',  ( -216.8640855513551458, 154.6031491089179610, 0.1911473656376749541 ) ) ;
#2724 = AXIS2_PLACEMENT_3D ( 'NONE', #7525, #11464, #5149 ) ;
#2725 = CARTESIAN_POINT ( 'NONE',  ( -179.1950877003932874, 117.8811570380880909, -0.5844242688643165318 ) ) ;
#2726 = FACE_OUTER_BOUND ( 'NONE', #6526, .T. ) ;
#2727 = ORIENTED_EDGE ( 'NONE', *, *, #9676, .F. ) ;
#2728 = EDGE_CURVE ( 'NONE', #4058, #9509, #5255, .T. ) ;
#2729 = CARTESIAN_POINT ( 'NONE',  ( -209.4369489341841586, 132.9646294043573675, 1.515400478619103763 ) ) ;
#2730 = CARTESIAN_POINT ( 'NONE',  ( 191.4227524587821279, 39.61567282607229856, -2.929995994935606252 ) ) ;
#2731 = EDGE_LOOP ( 'NONE', ( #5610, #5692, #13217, #779 ) ) ;
#2732 = VERTEX_POINT ( 'NONE', #913 ) ;
#2733 = VECTOR ( 'NONE', #9153, 1000.000000000000000 ) ;
#2734 = CARTESIAN_POINT ( 'NONE',  ( 0.7145311798161593231, -4.618802153517259867, -7.999999999999979572 ) ) ;
#2735 = CARTESIAN_POINT ( 'NONE',  ( -5.196152422706636465, 9.000000000000001776, 5.000000000000000000 ) ) ;
#2736 = EDGE_CURVE ( 'NONE', #11943, #13605, #2429, .T. ) ;
#2737 = DIRECTION ( 'NONE',  ( 1.000000000000000000, 0.000000000000000000, 0.000000000000000000 ) ) ;
#2738 = AXIS2_PLACEMENT_3D ( 'NONE', #5260, #4304, #9144 ) ;
#2739 = CARTESIAN_POINT ( 'NONE',  ( 190.0000000000000568, -179.3058001507315566, -30.31842631998718574 ) ) ;
#2740 = CARTESIAN_POINT ( 'NONE',  ( 172.5293059057019889, 61.25683321636181233, 10.00000000000000178 ) ) ;
#2741 = VECTOR ( 'NONE', #13587, 1000.000000000000000 ) ;
#2742 = CARTESIAN_POINT ( 'NONE',  ( -175.8063512637129975, 129.6626919947313468, 7.909502539118761888 ) ) ;
#2743 = CARTESIAN_POINT ( 'NONE',  ( -64.00000000000002842, -179.3058001507315566, -17.76585208085566947 ) ) ;
#2744 = CYLINDRICAL_SURFACE ( 'NONE', #15165, 1.499999999999997780 ) ;
#2745 = PRODUCT_DEFINITION_FORMATION_WITH_SPECIFIED_SOURCE ( 'ANY', '', #827, .NOT_KNOWN. ) ;
#2746 = VERTEX_POINT ( 'NONE', #11432 ) ;
#2747 = DIRECTION ( 'NONE',  ( 0.000000000000000000, -1.000000000000000000, -6.938893903907227145E-17 ) ) ;
#2748 = AXIS2_PLACEMENT_3D ( 'NONE', #12654, #6685, #5324 ) ;
#2749 = EDGE_CURVE ( 'NONE', #13177, #8794, #3687, .T. ) ;
#2750 = ORIENTED_EDGE ( 'NONE', *, *, #5008, .F. ) ;
#2751 = EDGE_LOOP ( 'NONE', ( #250, #275, #8439, #15379 ) ) ;
#2752 = LINE ( 'NONE', #11200, #9169 ) ;
#2753 = DIRECTION ( 'NONE',  ( 0.5000000000000001110, -0.8660254037844385966, 0.000000000000000000 ) ) ;
#2754 = LINE ( 'NONE', #13547, #6102 ) ;
#2755 = DIRECTION ( 'NONE',  ( -0.000000000000000000, 1.000000000000000000, -0.000000000000000000 ) ) ;
#2756 = DIRECTION ( 'NONE',  ( 0.000000000000000000, -1.000000000000000000, -4.956352788505162775E-17 ) ) ;
#2757 = DIRECTION ( 'NONE',  ( 1.000000000000000000, -0.000000000000000000, -0.000000000000000000 ) ) ;
#2758 = CARTESIAN_POINT ( 'NONE',  ( -215.0595991585972513, 153.5311831015895052, 5.434754235172610137 ) ) ;
#2759 = TOROIDAL_SURFACE ( 'NONE', #1438, 1.000000000000000000, 0.5000000000000000000 ) ;
#2760 = EDGE_LOOP ( 'NONE', ( #481, #636, #11539, #11295 ) ) ;
#2761 = CARTESIAN_POINT ( 'NONE',  ( 0.000000000000000000, 2.381569860407203532, -1.375000000000002665 ) ) ;
#2762 = CARTESIAN_POINT ( 'NONE',  ( -76.50000000000004263, 16.03993994372673626, 52.49999999999997868 ) ) ;
#2763 = CARTESIAN_POINT ( 'NONE',  ( -223.4350041415068802, 146.9203294941767979, 7.065198963530563425 ) ) ;
#2764 = ORIENTED_EDGE ( 'NONE', *, *, #13266, .T. ) ;
#2765 = AXIS2_PLACEMENT_3D ( 'NONE', #2957, #7779, #12567 ) ;
#2766 = EDGE_CURVE ( 'NONE', #1572, #4643, #12131, .T. ) ;
#2767 = AXIS2_PLACEMENT_3D ( 'NONE', #14539, #14465, #5005 ) ;
#2768 = CARTESIAN_POINT ( 'NONE',  ( -217.3957880433649450, 153.6844344254827490, 6.840999781109323052 ) ) ;
#2770 = EDGE_CURVE ( 'NONE', #13816, #5538, #14017, .T. ) ;
#2769 = EDGE_CURVE ( 'NONE', #2533, #9826, #15516, .T. ) ;
#2771 = EDGE_LOOP ( 'NONE', ( #6205, #9640, #7848, #6477 ) ) ;
#2772 = CARTESIAN_POINT ( 'NONE',  ( -169.1985897318295144, 125.0868387319165862, -3.803836676538010497 ) ) ;
#2773 = CARTESIAN_POINT ( 'NONE',  ( 188.3535365708562779, 39.18556319200014570, -2.939344140512093251 ) ) ;
#2774 = CIRCLE ( 'NONE', #11846, 1.499999999999988232 ) ;
#2775 = ORIENTED_EDGE ( 'NONE', *, *, #1077, .F. ) ;
#2776 = DIRECTION ( 'NONE',  ( -0.000000000000000000, -0.000000000000000000, 1.000000000000000000 ) ) ;
#2777 = CARTESIAN_POINT ( 'NONE',  ( 184.0000000000000568, 15.53993994372673981, -12.49999999999999289 ) ) ;
#2778 = AXIS2_PLACEMENT_3D ( 'NONE', #15501, #4698, #4460 ) ;
#2779 = CYLINDRICAL_SURFACE ( 'NONE', #9655, 1.499999999999994449 ) ;
#2780 = ORIENTED_EDGE ( 'NONE', *, *, #4665, .F. ) ;
#2781 = VECTOR ( 'NONE', #11909, 1000.000000000000000 ) ;
#2782 = CONICAL_SURFACE ( 'NONE', #10587, 3.524999999999998579, 0.7853981633974482790 ) ;
#2783 = CARTESIAN_POINT ( 'NONE',  ( 184.0000000000000568, -177.3058001507315566, -41.45141194869120227 ) ) ;
#2784 = ORIENTED_EDGE ( 'NONE', *, *, #7217, .T. ) ;
#2785 = CYLINDRICAL_SURFACE ( 'NONE', #15558, 1.500000000000000444 ) ;
#2786 = ORIENTED_EDGE ( 'NONE', *, *, #6303, .T. ) ;
#2787 = LINE ( 'NONE', #11078, #7974 ) ;
#2788 = PLANE ( 'NONE',  #3260 ) ;
#2789 = CIRCLE ( 'NONE', #13612, 3.499999999999999556 ) ;
#2790 = EDGE_LOOP ( 'NONE', ( #5117, #15465 ) ) ;
#2791 = EDGE_LOOP ( 'NONE', ( #13497, #12888, #1976, #8409, #9800, #11347, #11896, #12895, #10326, #8554, #14802, #14242, #5073, #13272, #96, #7229, #10930 ) ) ;
#2792 = LINE ( 'NONE', #7617, #5517 ) ;
#2793 = CARTESIAN_POINT ( 'NONE',  ( 202.9147226314038051, 48.88641379461363101, -0.9068510277452211943 ) ) ;
#2794 = AXIS2_PLACEMENT_3D ( 'NONE', #9407, #2511, #6227 ) ;
#2795 = ORIENTED_EDGE ( 'NONE', *, *, #10101, .F. ) ;
#2796 = TOROIDAL_SURFACE ( 'NONE', #5053, 1.000000000000000000, 0.5000000000000000000 ) ;
#2797 = DIRECTION ( 'NONE',  ( -0.000000000000000000, -0.000000000000000000, 1.000000000000000000 ) ) ;
#2798 = EDGE_CURVE ( 'NONE', #85, #7982, #2179, .T. ) ;
#2799 = DIRECTION ( 'NONE',  ( -0.000000000000000000, -1.000000000000000000, -0.000000000000000000 ) ) ;
#2800 = FACE_OUTER_BOUND ( 'NONE', #1018, .T. ) ;
#2801 = CARTESIAN_POINT ( 'NONE',  ( 0.000000000000000000, 0.000000000000000000, 0.000000000000000000 ) ) ;
#2802 = AXIS2_PLACEMENT_3D ( 'NONE', #14369, #9570, #2303 ) ;
#2803 = CONICAL_SURFACE ( 'NONE', #2289, 3.525000000000000355, 0.7853981633974482790 ) ;
#2804 = EDGE_CURVE ( 'NONE', #2947, #6121, #12506, .T. ) ;
#2805 = PLANE ( 'NONE',  #14917 ) ;
#2806 = VERTEX_POINT ( 'NONE', #4709 ) ;
#2807 = FACE_OUTER_BOUND ( 'NONE', #9112, .T. ) ;
#2808 = CARTESIAN_POINT ( 'NONE',  ( -217.5843001957448450, 153.3500559703123827, -2.470211307036358495 ) ) ;
#2809 = CARTESIAN_POINT ( 'NONE',  ( -211.5558396979514839, 139.0314540006070274, -4.642206099735020963 ) ) ;
#2810 = CARTESIAN_POINT ( 'NONE',  ( -64.00000000000002842, 16.03993994372673981, 24.94742576086838781 ) ) ;
#2811 = ORIENTED_EDGE ( 'NONE', *, *, #1880, .F. ) ;
#2812 = CARTESIAN_POINT ( 'NONE',  ( -193.5534063424729254, 128.8169105028637205, 7.918248976830644992 ) ) ;
#2813 = CARTESIAN_POINT ( 'NONE',  ( 202.8187013049204950, 32.78779105710274422, -6.518094968334741779 ) ) ;
#2814 = VERTEX_POINT ( 'NONE', #2264 ) ;
#2815 = VECTOR ( 'NONE', #12122, 1000.000000000000000 ) ;
#2816 = DIRECTION ( 'NONE',  ( -0.000000000000000000, -0.000000000000000000, 1.000000000000000000 ) ) ;
#2817 = PLANE ( 'NONE',  #3939 ) ;
#2818 = PRESENTATION_LAYER_ASSIGNMENT (  '', '', ( #1288 ) ) ;
#2819 = CARTESIAN_POINT ( 'NONE',  ( 190.0000000000000568, 15.03993994372673981, -3.075184203610571654 ) ) ;
#2820 = ADVANCED_FACE ( 'NONE', ( #14486 ), #2347, .T. ) ;
#2821 = DIRECTION ( 'NONE',  ( -0.8731965799097685110, 0.4873681696970816324, 0.000000000000000000 ) ) ;
#2822 = EDGE_LOOP ( 'NONE', ( #3197, #10041, #9471, #12428 ) ) ;
#2823 = CIRCLE ( 'NONE', #1287, 1.699999999999996625 ) ;
#2824 = DIRECTION ( 'NONE',  ( 0.000000000000000000, -1.000000000000000000, -1.156482317317871478E-16 ) ) ;
#2825 = CARTESIAN_POINT ( 'NONE',  ( -188.0905678060899220, 138.5068454852687125, 5.434754235172603920 ) ) ;
#2826 = CARTESIAN_POINT ( 'NONE',  ( 215.4200305399390345, 33.33196348269225240, 0.000000000000000000 ) ) ;
#2827 = VECTOR ( 'NONE', #14128, 1000.000000000000000 ) ;
#2828 = FACE_OUTER_BOUND ( 'NONE', #8438, .T. ) ;
#2829 = ORIENTED_EDGE ( 'NONE', *, *, #2573, .F. ) ;
#2830 = CARTESIAN_POINT ( 'NONE',  ( 64.00000000000005684, 59.53993994372674337, 15.00000000000070166 ) ) ;
#2831 = ORIENTED_EDGE ( 'NONE', *, *, #14143, .F. ) ;
#2832 = ORIENTED_EDGE ( 'NONE', *, *, #14560, .F. ) ;
#2833 = PLANE ( 'NONE',  #5632 ) ;
#2834 = CARTESIAN_POINT ( 'NONE',  ( 184.0000000000000568, 17.53993994372673271, 48.99999999999997158 ) ) ;
#2835 =( NAMED_UNIT ( * ) SI_UNIT ( $, .STERADIAN. ) SOLID_ANGLE_UNIT ( ) );
#2836 = CARTESIAN_POINT ( 'NONE',  ( 6.399999999999999467, 4.618802153516981868, -7.999999999999979572 ) ) ;
#2837 = STYLED_ITEM ( 'NONE', ( #13045 ), #10736 ) ;
#2838 = CARTESIAN_POINT ( 'NONE',  ( -220.0166125838651681, 153.0449145666497657, -1.086335426908857871 ) ) ;
#2839 = CARTESIAN_POINT ( 'NONE',  ( -202.9262818645171649, 144.6968105762408072, 7.919662025281898998 ) ) ;
#2840 = AXIS2_PLACEMENT_3D ( 'NONE', #9711, #4723, #3545 ) ;
#2841 = ORIENTED_EDGE ( 'NONE', *, *, #14264, .F. ) ;
#2842 = ADVANCED_FACE ( 'NONE', ( #7097 ), #9616, .T. ) ;
#2843 = PRODUCT_DEFINITION_CONTEXT ( 'detailed design', #12900, 'design' ) ;
#2844 = DIRECTION ( 'NONE',  ( -1.000000000000000000, 0.000000000000000000, -0.000000000000000000 ) ) ;
#2845 = CARTESIAN_POINT ( 'NONE',  ( 0.2456200930618607225, 1.587713240271468207, -2.750000000000000000 ) ) ;
#2846 = CARTESIAN_POINT ( 'NONE',  ( -224.6003591769690502, 144.8324130182638783, 2.185988691727169808 ) ) ;
#2847 = ORIENTED_EDGE ( 'NONE', *, *, #13348, .T. ) ;
#2848 = CARTESIAN_POINT ( 'NONE',  ( -221.9533209457892156, 149.5749975243766130, 9.934841322514504469 ) ) ;
#2849 = EDGE_LOOP ( 'NONE', ( #8044, #1302, #12370, #2119 ) ) ;
#2850 = CARTESIAN_POINT ( 'NONE',  ( 184.0000000000000568, 17.53993994372673981, -12.49999999999999467 ) ) ;
#2851 = CIRCLE ( 'NONE', #4345, 5.000000000000000000 ) ;
#2852 = CARTESIAN_POINT ( 'NONE',  ( 209.6082252582704371, 33.74895655718308518, -4.813932606105665535 ) ) ;
#2853 = ORIENTED_EDGE ( 'NONE', *, *, #5443, .F. ) ;
#2854 = DIRECTION ( 'NONE',  ( -0.000000000000000000, -0.000000000000000000, 1.000000000000000000 ) ) ;
#2855 = DIRECTION ( 'NONE',  ( 0.000000000000000000, 0.000000000000000000, 1.000000000000000000 ) ) ;
#2856 = ADVANCED_FACE ( 'NONE', ( #7256 ), #10005, .T. ) ;
#2857 = DIRECTION ( 'NONE',  ( -0.000000000000000000, -0.000000000000000000, 1.000000000000000000 ) ) ;
#2858 = ORIENTED_EDGE ( 'NONE', *, *, #12469, .T. ) ;
#2859 = EDGE_CURVE ( 'NONE', #8410, #11968, #3608, .T. ) ;
#2860 = APPLICATION_PROTOCOL_DEFINITION ( 'draft international standard', 'automotive_design', 1998, #14795 ) ;
#2861 = VERTEX_POINT ( 'NONE', #110 ) ;
#2862 = AXIS2_PLACEMENT_3D ( 'NONE', #14971, #2686, #6480 ) ;
#2863 = CARTESIAN_POINT ( 'NONE',  ( 20.91029453487719181, 40.04259805664093363, 10.00000000000000178 ) ) ;
#2864 = ADVANCED_FACE ( 'NONE', ( #8443 ), #11902, .T. ) ;
#2865 = CARTESIAN_POINT ( 'NONE',  ( -155.8510687235160219, 110.8158223976909369, 9.813105602333695998 ) ) ;
#2866 = VERTEX_POINT ( 'NONE', #3453 ) ;
#2867 = CARTESIAN_POINT ( 'NONE',  ( 194.0000000000000568, 59.53993994372674337, 20.00000000000000355 ) ) ;
#2868 = MECHANICAL_DESIGN_GEOMETRIC_PRESENTATION_REPRESENTATION (  '', ( #11186 ), #5388 ) ;
#2869 = FACE_OUTER_BOUND ( 'NONE', #5166, .T. ) ;
#2870 = ORIENTED_EDGE ( 'NONE', *, *, #1625, .F. ) ;
#2871 = ORIENTED_EDGE ( 'NONE', *, *, #4683, .F. ) ;
#2872 = DIRECTION ( 'NONE',  ( -1.000000000000000000, -0.000000000000000000, -0.000000000000000000 ) ) ;
#2873 = CARTESIAN_POINT ( 'NONE',  ( 203.1427736312160164, 48.80054947466439330, -2.493724563924679671 ) ) ;
#2874 = ORIENTED_EDGE ( 'NONE', *, *, #3740, .T. ) ;
#2875 = DIRECTION ( 'NONE',  ( -0.000000000000000000, 1.000000000000000000, 0.000000000000000000 ) ) ;
#2876 = DIRECTION ( 'NONE',  ( 5.518327896226369609E-17, -0.9902680687415712502, -0.1391731009600584990 ) ) ;
#2877 = CARTESIAN_POINT ( 'NONE',  ( -108.0000000000000568, 59.53993994372674337, 20.00000000000000355 ) ) ;
#2878 = CARTESIAN_POINT ( 'NONE',  ( -222.5463326935617658, 144.4088500683630514, 2.431557144026069928 ) ) ;
#2879 = CARTESIAN_POINT ( 'NONE',  ( 184.0000000000000568, 17.53993994372673981, -13.99999999999999112 ) ) ;
#2880 = EDGE_CURVE ( 'NONE', #14289, #6589, #991, .T. ) ;
#2881 = AXIS2_PLACEMENT_3D ( 'NONE', #13610, #12578, #412 ) ;
#2882 = EDGE_CURVE ( 'NONE', #11790, #2386, #5470, .T. ) ;
#2883 = DIRECTION ( 'NONE',  ( 1.000000000000000000, 0.000000000000000000, 0.000000000000000000 ) ) ;
#2884 = ORIENTED_EDGE ( 'NONE', *, *, #4665, .T. ) ;
#2885 = CARTESIAN_POINT ( 'NONE',  ( 170.8293059057019718, 61.25683321636181233, 5.000000000000000000 ) ) ;
#2886 = CARTESIAN_POINT ( 'NONE',  ( -216.6959657076304211, 154.8907008763735291, 2.027593286600615219 ) ) ;
#2887 = CIRCLE ( 'NONE', #9443, 54.67486482576605766 ) ;
#2888 = CARTESIAN_POINT ( 'NONE',  ( -213.7219974575431252, 137.2233070386400584, -2.964974570226852180 ) ) ;
#2889 = DIRECTION ( 'NONE',  ( -0.000000000000000000, -0.000000000000000000, -1.000000000000000000 ) ) ;
#2890 = ORIENTED_EDGE ( 'NONE', *, *, #10778, .T. ) ;
#2891 = CARTESIAN_POINT ( 'NONE',  ( -225.7548303624724610, 142.7639966680278576, 1.446957622915672204 ) ) ;
#2892 = CARTESIAN_POINT ( 'NONE',  ( 208.8213467238098247, 41.99652926550911758, -5.863399402755005596 ) ) ;
#2893 = VECTOR ( 'NONE', #6015, 1000.000000000000000 ) ;
#2894 = ORIENTED_EDGE ( 'NONE', *, *, #1115, .F. ) ;
#2895 = ADVANCED_FACE ( 'NONE', ( #1227 ), #5821, .F. ) ;
#2896 = FACE_OUTER_BOUND ( 'NONE', #5305, .T. ) ;
#2897 = FACE_OUTER_BOUND ( 'NONE', #6854, .T. ) ;
#2898 = CARTESIAN_POINT ( 'NONE',  ( -171.4541674549778918, 121.0456171749203662, 2.431557144026069928 ) ) ;
#2899 = AXIS2_PLACEMENT_3D ( 'NONE', #9214, #14011, #8036 ) ;
#2900 = DIRECTION ( 'NONE',  ( 0.000000000000000000, 0.000000000000000000, 1.000000000000000000 ) ) ;
#2901 = CARTESIAN_POINT ( 'NONE',  ( -35.99999999999995026, 64.53993994372673626, 15.00000000000139977 ) ) ;
#2902 = EDGE_LOOP ( 'NONE', ( #10350, #2462 ) ) ;
#2903 = DIRECTION ( 'NONE',  ( -0.000000000000000000, -0.000000000000000000, -1.000000000000000000 ) ) ;
#2904 = CARTESIAN_POINT ( 'NONE',  ( -192.1748460459477030, 141.1892528453990110, 3.478855109513427468 ) ) ;
#2905 = DIRECTION ( 'NONE',  ( 1.000000000000000000, 0.000000000000000000, 0.000000000000000000 ) ) ;
#2906 = CARTESIAN_POINT ( 'NONE',  ( -155.6477983077465126, 110.3277548344292995, -4.884442077755424272 ) ) ;
#2907 = EDGE_LOOP ( 'NONE', ( #5248, #13337, #5877, #13560 ) ) ;
#2908 = DIRECTION ( 'NONE',  ( 0.000000000000000000, 0.000000000000000000, -1.000000000000000000 ) ) ;
#2909 = AXIS2_PLACEMENT_3D ( 'NONE', #7942, #5322, #5486 ) ;
#2910 = EDGE_LOOP ( 'NONE', ( #3757, #8169, #4486, #15269 ) ) ;
#2911 = EDGE_CURVE ( 'NONE', #5528, #12980, #7333, .T. ) ;
#2912 = VERTEX_POINT ( 'NONE', #8215 ) ;
#2913 = DIRECTION ( 'NONE',  ( -0.7071067811864983899, 8.659560562354331352E-17, 0.7071067811865966446 ) ) ;
#2914 = DIRECTION ( 'NONE',  ( -1.000000000000000000, 0.000000000000000000, 0.000000000000000000 ) ) ;
#2915 = CARTESIAN_POINT ( 'NONE',  ( 224.0000000000000853, 59.53993994372674337, 25.00000000000000000 ) ) ;
#2916 = CARTESIAN_POINT ( 'NONE',  ( 14.00000000000004086, 64.53993994372673626, 18.50000000000105160 ) ) ;
#2917 = DIRECTION ( 'NONE',  ( 0.000000000000000000, 0.000000000000000000, 1.000000000000000000 ) ) ;
#2918 = CARTESIAN_POINT ( 'NONE',  ( -216.7216729069046437, 154.8463875879167801, 3.280095325655319805 ) ) ;
#2919 = ORIENTED_EDGE ( 'NONE', *, *, #11934, .T. ) ;
#2920 = AXIS2_PLACEMENT_3D ( 'NONE', #8486, #15402, #4602 ) ;
#2921 = CARTESIAN_POINT ( 'NONE',  ( 0.1090894304641068929, 1.847874265840319330, -2.299387885565524758 ) ) ;
#2922 = DIRECTION ( 'NONE',  ( -0.000000000000000000, 0.000000000000000000, 1.000000000000000000 ) ) ;
#2923 = CARTESIAN_POINT ( 'NONE',  ( 208.8002188652075972, 39.64064887424692785, -1.560527519332197022 ) ) ;
#2924 = EDGE_CURVE ( 'NONE', #7800, #12461, #9498, .T. ) ;
#2925 = CARTESIAN_POINT ( 'NONE',  ( -224.3577192346544109, 145.2671405629664605, 0.1302923617619599905 ) ) ;
#2926 = ORIENTED_EDGE ( 'NONE', *, *, #9479, .T. ) ;
#2928 = B_SPLINE_CURVE_WITH_KNOTS ( 'NONE', 3,
 ( #4531, #9359, #15411, #1848, #5722, #732 ),
 .UNSPECIFIED., .F., .F.,
 ( 4, 2, 4 ),
 ( 0.001606744326298686649, 0.002406996759593248332, 0.003207249192887810449 ),
 .UNSPECIFIED. ) ;
#2927 = CARTESIAN_POINT ( 'NONE',  ( -219.9692141781003443, 153.1298362508722448, 5.829181591414630326 ) ) ;
#2929 = VERTEX_POINT ( 'NONE', #8284 ) ;
#2930 = CARTESIAN_POINT ( 'NONE',  ( -172.0842878089050600, 119.9166576486493057, -4.812951232078420460 ) ) ;
#2931 = DIRECTION ( 'NONE',  ( 1.000000000000000000, 0.000000000000000000, 0.000000000000000000 ) ) ;
#2932 = AXIS2_PLACEMENT_3D ( 'NONE', #8083, #5923, #14282 ) ;
#2933 = ORIENTED_EDGE ( 'NONE', *, *, #1234, .F. ) ;
#2934 = CYLINDRICAL_SURFACE ( 'NONE', #5413, 0.5000000000000004441 ) ;
#2935 = CARTESIAN_POINT ( 'NONE',  ( 0.4964154566687820624, 8.859816792613631975, -0.6543471694412253958 ) ) ;
#2936 = VECTOR ( 'NONE', #10232, 1000.000000000000000 ) ;
#2937 = DIRECTION ( 'NONE',  ( 0.000000000000000000, -1.000000000000000000, 0.000000000000000000 ) ) ;
#2939 = VERTEX_POINT ( 'NONE', #5181 ) ;
#2938 = EDGE_CURVE ( 'NONE', #1447, #1126, #13504, .T. ) ;
#2940 = ORIENTED_EDGE ( 'NONE', *, *, #11588, .F. ) ;
#2941 = CARTESIAN_POINT ( 'NONE',  ( 190.0000000000000568, -178.8058001507315566, 52.19066787724494816 ) ) ;
#2942 = EDGE_LOOP ( 'NONE', ( #2870, #2121, #10598, #12745 ) ) ;
#2943 = DIRECTION ( 'NONE',  ( 0.000000000000000000, 0.000000000000000000, -1.000000000000000000 ) ) ;
#2944 = AXIS2_PLACEMENT_3D ( 'NONE', #6456, #5104, #11261 ) ;
#2945 = LINE ( 'NONE', #10130, #1482 ) ;
#2946 = ORIENTED_EDGE ( 'NONE', *, *, #9969, .F. ) ;
#2947 = VERTEX_POINT ( 'NONE', #13532 ) ;
#2948 = DIRECTION ( 'NONE',  ( 1.000000000000000000, 0.000000000000000000, 0.000000000000000000 ) ) ;
#2949 = DIRECTION ( 'NONE',  ( -1.000000000000000000, 0.000000000000000000, 0.000000000000000000 ) ) ;
#2950 = ADVANCED_FACE ( 'NONE', ( #14790 ), #4437, .F. ) ;
#2951 = ORIENTED_EDGE ( 'NONE', *, *, #5707, .T. ) ;
#2952 = CARTESIAN_POINT ( 'NONE',  ( -76.00000000000001421, -178.8058001507315566, 52.19066787724494816 ) ) ;
#2953 = FACE_OUTER_BOUND ( 'NONE', #8679, .T. ) ;
#2954 = DIRECTION ( 'NONE',  ( 1.000000000000000000, -2.751328491981765035E-32, 3.965082230804130220E-16 ) ) ;
#2955 = CYLINDRICAL_SURFACE ( 'NONE', #8999, 1.700000000000001954 ) ;
#2956 = CARTESIAN_POINT ( 'NONE',  ( -34.79899788034579444, 48.72489408690345414, 10.00000000000000178 ) ) ;
#2957 = CARTESIAN_POINT ( 'NONE',  ( 224.0000000000000853, 26.39124795404934076, 0.000000000000000000 ) ) ;
#2958 = VERTEX_POINT ( 'NONE', #493 ) ;
#2959 = PLANE ( 'NONE',  #4066 ) ;
#2960 = DIRECTION ( 'NONE',  ( 1.000000000000000000, 0.000000000000000000, 0.000000000000000000 ) ) ;
#2961 = CARTESIAN_POINT ( 'NONE',  ( -214.8672114436478466, 153.8753479842104355, 1.515441477536284998 ) ) ;
#2962 = ORIENTED_EDGE ( 'NONE', *, *, #5310, .T. ) ;
#2963 = CARTESIAN_POINT ( 'NONE',  ( -179.1973253475678121, 117.8771479419235675, 5.305259944336949474 ) ) ;
#2964 = UNCERTAINTY_MEASURE_WITH_UNIT (LENGTH_MEASURE( 1.000000000000000082E-05 ), #13235, 'distance_accuracy_value', 'NONE');
#2965 = CARTESIAN_POINT ( 'NONE',  ( 208.8276044750562335, 41.97590694738037342, -2.864603354092789100 ) ) ;
#2966 = ORIENTED_EDGE ( 'NONE', *, *, #13201, .F. ) ;
#2967 = EDGE_CURVE ( 'NONE', #12864, #2654, #10754, .T. ) ;
#2968 = ADVANCED_FACE ( 'NONE', ( #12508, #12432, #8590 ), #3983, .F. ) ;
#2969 = CARTESIAN_POINT ( 'NONE',  ( 17.41029453487719181, 40.04259805664093363, 5.000000000000000000 ) ) ;
#2970 = DIRECTION ( 'NONE',  ( 5.518327896226364679E-17, 0.9902680687415713612, -0.1391731009600582492 ) ) ;
#2971 = DIRECTION ( 'NONE',  ( 0.000000000000000000, -4.956352788505162775E-17, 1.000000000000000000 ) ) ;
#2972 = CIRCLE ( 'NONE', #10288, 1.700000000000000178 ) ;
#2973 = DIRECTION ( 'NONE',  ( 0.000000000000000000, 0.000000000000000000, 1.000000000000000000 ) ) ;
#2974 = ORIENTED_EDGE ( 'NONE', *, *, #14811, .F. ) ;
#2975 = CYLINDRICAL_SURFACE ( 'NONE', #10213, 1.700000000000007061 ) ;
#2976 = CARTESIAN_POINT ( 'NONE',  ( -213.7333075327791789, 137.2030432634720967, 7.918248976830621011 ) ) ;
#2977 = DIRECTION ( 'NONE',  ( 0.000000000000000000, 0.000000000000000000, 1.000000000000000000 ) ) ;
#2978 = DIRECTION ( 'NONE',  ( 0.000000000000000000, 0.000000000000000000, 1.000000000000000000 ) ) ;
#2979 = B_SPLINE_SURFACE_WITH_KNOTS ( 'NONE', 3, 3, ( 
 ( #10821, #12000, #7118, #10979, #8387, #3703, #13322, #3627, #6236, #11048, #199, #13167, #2364, #5047, #8461, #9552, #5999 ),
 ( #1094, #5917, #4897, #14505, #10738, #4814, #2523, #7354, #12149, #6162, #4970, #9787, #12295, #14741, #10026, #9949, #288 ),
 ( #359, #2758, #3936, #1643, #1477, #5201, #14810, #13634, #12455, #12378, #1564, #7582, #14666, #8758, #13552, #4006, #8840 ),
 ( #11207, #5126, #6400, #3864, #2680, #2839, #7660, #6476, #8687, #13479, #7502, #6318, #11132, #13215, #2491, #2339, #3909 ),
 ( #5097, #1298, #14402, #3600, #13292, #4867, #6056, #13137, #5021, #2413, #13375, #7403, #3673, #8659, #11103, #257, #7248 ),
 ( #9921, #8507, #11974, #12042, #1215, #8583, #6131, #173, #8436, #13453, #9762, #7473, #1448, #12193, #12269, #7324, #12121 ),
 ( #11023, #6285, #7171, #1373, #3754, #15578, #1144, #10952, #4943, #9685, #10874, #28, #102, #4782, #14478, #6211, #9847 ),
 ( #2652, #14551, #9606, #2576, #5970, #14640, #3837, #14713, #10789, #2812, #14864, #573, #7790, #10001, #5411, #11181, #488 ),
 ( #13526, #15095, #11490, #650, #12500, #14783, #3977, #8895, #409, #1617, #8732, #10227, #13606, #8973, #2963, #4059, #4208 ),
 ( #5490, #7633, #8809, #10304, #13685, #7552, #12425, #6448, #4134, #1690, #11408, #11254, #9045, #5327, #3044, #12656, #12573 ),
 ( #2891, #7714, #15021, #6605, #1843, #2729, #1770, #14944, #333, #12350, #6527, #10151, #5246, #10071, #11327, #13766, #5174 ),
 ( #13845, #7873, #1534, #6687, #6370, #11795, #10461, #12731, #14075, #3269, #886, #3117, #8110, #12893, #13928, #4445, #9127 ),
 ( #11723, #10380, #5569, #10693, #3425, #14228, #6912, #5718, #5875, #7948, #1998, #14154, #2079, #2156, #1920, #6991, #15173 ),
 ( #964, #808, #12809, #7069, #8185, #10528, #5642, #4288, #4368, #3349, #5791, #8259, #11879, #15326, #4525, #9355, #6755 ),
 ( #12969, #10616, #15406, #15249, #4606, #8021, #9429, #11562, #725, #9278, #13034, #2235, #1051, #9204, #3191, #14001, #6836 ),
 ( #11646, #1127, #6267, #14618, #9824, #2469, #7303, #1432, #14300, #13193, #9744, #9666, #13354, #8335, #2557, #10770, #6033 ),
 ( #12025, #8417, #2634, #3733, #13273, #1194, #15484, #15556, #14536, #1355, #3818, #7456, #1280, #6113, #12101, #4679, #10 ),
 ( #8560, #7384, #10855, #87, #3581, #10932, #9507, #13120, #4848, #4927, #12177, #6194, #11006, #14384, #14461, #8638, #4761 ),
 ( #3499, #2319, #12252, #7149, #3655, #5948, #9584, #8491, #7231, #2396, #11955, #156, #5001, #13435, #5307, #1594, #6590 ),
 ( #13823, #316, #11162, #7854, #6430, #9903, #9983, #5156, #6507, #4040, #13744, #12330, #11390, #7693, #5392, #15002, #10134 ) ),
 .UNSPECIFIED., .T., .F., .F.,
 ( 4, 1, 1, 1, 1, 1, 1, 1, 2, 1, 1, 1, 1, 1, 1, 1, 4 ),
 ( 4, 2, 2, 2, 2, 2, 3, 4 ),
 ( 0.000000000000000000, 0.06231844716590150685, 0.1246368943318030137, 0.1869553414977045136, 0.2492737886636060274, 0.3115922358295075134, 0.3739106829954090272, 0.4362291301613105410, 0.4985475773272120548, 0.5612291301613105965, 0.6239106829954090827, 0.6865922358295075689, 0.7492737886636060551, 0.8119553414977045414, 0.8746368943318030276, 0.9373184471659015138, 1.000000000000000000 ),
 ( 0.000000000000000000, 0.2455027589669699362, 0.3041813370740077405, 0.5308033955276700855, 0.6372805264318514018, 0.8233339832829627003, 1.000000000000000000, 1.166726064904226812 ),
 .UNSPECIFIED. ) ;
#2980 = EDGE_LOOP ( 'NONE', ( #8266, #12008, #4748, #7928, #7781, #10017, #1254, #1301, #11027, #12713, #5802, #4416, #8024, #15559, #151, #9887, #4018 ) ) ;
#2981 = FACE_BOUND ( 'NONE', #12391, .T. ) ;
#2982 = AXIS2_PLACEMENT_3D ( 'NONE', #5268, #12522, #122 ) ;
#2983 = ORIENTED_EDGE ( 'NONE', *, *, #14542, .T. ) ;
#2984 = VERTEX_POINT ( 'NONE', #4065 ) ;
#2985 = DIRECTION ( 'NONE',  ( -1.000000000000000000, -0.000000000000000000, 0.000000000000000000 ) ) ;
#2986 = CARTESIAN_POINT ( 'NONE',  ( 194.0000000000000568, 64.53993994372673626, 10.00000000000000178 ) ) ;
#2987 = AXIS2_PLACEMENT_3D ( 'NONE', #6893, #5770, #10596 ) ;
#2988 = CIRCLE ( 'NONE', #2482, 6.999999999999992006 ) ;
#2989 = CARTESIAN_POINT ( 'NONE',  ( -172.2044971521971490, 119.7012837404576260, 9.318491256855141458 ) ) ;
#2990 = CARTESIAN_POINT ( 'NONE',  ( -218.5136094644957723, 155.7377805866632627, 0.8972885290472901731 ) ) ;
#2991 = DIRECTION ( 'NONE',  ( 1.000000000000000000, -0.000000000000000000, -0.000000000000000000 ) ) ;
#2992 = AXIS2_PLACEMENT_3D ( 'NONE', #2068, #11921, #15610 ) ;
#2993 = DIRECTION ( 'NONE',  ( -0.000000000000000000, 0.000000000000000000, 1.000000000000000000 ) ) ;
#2994 = CARTESIAN_POINT ( 'NONE',  ( 185.1062858801516882, 25.86394065090268057, 18.00000000000000355 ) ) ;
#2995 = VECTOR ( 'NONE', #11739, 1000.000000000000000 ) ;
#2996 = EDGE_CURVE ( 'NONE', #13828, #3648, #1540, .T. ) ;
#2997 = CARTESIAN_POINT ( 'NONE',  ( 194.7891036845171300, 47.85977741052224133, -6.433373108600371815 ) ) ;
#2998 = CARTESIAN_POINT ( 'NONE',  ( -220.1893657699865230, 152.7354001160375674, -1.484330510406285830 ) ) ;
#2999 = ORIENTED_EDGE ( 'NONE', *, *, #3303, .T. ) ;
#3000 = CARTESIAN_POINT ( 'NONE',  ( -219.4227507837628366, 154.1089112020831635, 7.576492947193309568 ) ) ;
#3001 = ORIENTED_EDGE ( 'NONE', *, *, #14701, .T. ) ;
#3002 = DIRECTION ( 'NONE',  ( 0.000000000000000000, 0.000000000000000000, -1.000000000000000000 ) ) ;
#3003 = DIRECTION ( 'NONE',  ( -0.000000000000000000, 1.486905836551548832E-16, -1.000000000000000000 ) ) ;
#3004 = ORIENTED_EDGE ( 'NONE', *, *, #7863, .F. ) ;
#3005 = CARTESIAN_POINT ( 'NONE',  ( 170.8293059057019718, 61.25683321636181233, 7.600000000000002309 ) ) ;
#3006 = DIRECTION ( 'NONE',  ( 0.000000000000000000, 0.000000000000000000, 1.000000000000000000 ) ) ;
#3007 = VECTOR ( 'NONE', #11348, 1000.000000000000114 ) ;
#3008 = VECTOR ( 'NONE', #70, 1000.000000000000000 ) ;
#3009 = AXIS2_PLACEMENT_3D ( 'NONE', #13350, #10767, #15553 ) ;
#3010 = DIRECTION ( 'NONE',  ( 0.000000000000000000, 0.000000000000000000, -1.000000000000000000 ) ) ;
#3011 = ORIENTED_EDGE ( 'NONE', *, *, #362, .T. ) ;
#3012 = ORIENTED_EDGE ( 'NONE', *, *, #11091, .F. ) ;
#3013 = B_SPLINE_CURVE_WITH_KNOTS ( 'NONE', 3,
 ( #14159, #8194, #2161, #6995, #2240, #14699 ),
 .UNSPECIFIED., .F., .F.,
 ( 4, 2, 4 ),
 ( 0.009986348756006662580, 0.01078976120410690340, 0.01159317365220714248 ),
 .UNSPECIFIED. ) ;
#3014 = CIRCLE ( 'NONE', #9074, 8.000000000000028422 ) ;
#3015 = CARTESIAN_POINT ( 'NONE',  ( 192.9601959511087728, 50.37386974367067438, -4.870874480120333416 ) ) ;
#3016 = DIRECTION ( 'NONE',  ( 0.000000000000000000, 0.000000000000000000, 1.000000000000000000 ) ) ;
#3017 = EDGE_LOOP ( 'NONE', ( #8521, #14268, #10102, #885 ) ) ;
#3019 = CIRCLE ( 'NONE', #13582, 335.5619230110239641 ) ;
#3018 = FACE_OUTER_BOUND ( 'NONE', #708, .T. ) ;
#3020 = LINE ( 'NONE', #465, #8570 ) ;
#3021 = ORIENTED_EDGE ( 'NONE', *, *, #4796, .T. ) ;
#3022 = EDGE_LOOP ( 'NONE', ( #13945, #5116, #1889, #5091, #12792 ) ) ;
#3023 = FACE_OUTER_BOUND ( 'NONE', #9962, .T. ) ;
#3024 = ADVANCED_FACE ( 'NONE', ( #3915 ), #341, .F. ) ;
#3025 = DIRECTION ( 'NONE',  ( -0.000000000000000000, 0.9902680687415711391, -0.1391731009600603308 ) ) ;
#3026 = VERTEX_POINT ( 'NONE', #2585 ) ;
#3027 = CARTESIAN_POINT ( 'NONE',  ( 205.4496313998743915, 47.84832575209421890, -7.060263518810960370 ) ) ;
#3028 = LINE ( 'NONE', #15083, #2021 ) ;
#3029 = AXIS2_PLACEMENT_3D ( 'NONE', #14409, #2420, #7253 ) ;
#3030 = STYLED_ITEM ( 'NONE', ( #5938 ), #11070 ) ;
#3031 = DIRECTION ( 'NONE',  ( -0.000000000000000000, 0.000000000000000000, 1.000000000000000000 ) ) ;
#3032 = FACE_OUTER_BOUND ( 'NONE', #1952, .T. ) ;
#3033 = CARTESIAN_POINT ( 'NONE',  ( 200.1062858801516597, 40.86394065090267702, 18.00000000000000355 ) ) ;
#3034 = AXIS2_PLACEMENT_3D ( 'NONE', #477, #7623, #11089 ) ;
#3035 = ADVANCED_FACE ( 'NONE', ( #13611 ), #2817, .F. ) ;
#3036 = DIRECTION ( 'NONE',  ( 0.000000000000000000, 0.000000000000000000, 1.000000000000000000 ) ) ;
#3037 = CIRCLE ( 'NONE', #5050, 3.500000000000003109 ) ;
#3038 = ORIENTED_EDGE ( 'NONE', *, *, #12446, .T. ) ;
#3039 = CARTESIAN_POINT ( 'NONE',  ( 175.9483885134608272, -179.3058001507315566, 84.88378295107887084 ) ) ;
#3040 = CARTESIAN_POINT ( 'NONE',  ( -177.5434268683390826, 132.5922366007948199, -0.4547266291960713747 ) ) ;
#3041 = VECTOR ( 'NONE', #11189, 1000.000000000000000 ) ;
#3042 = FACE_OUTER_BOUND ( 'NONE', #467, .T. ) ;
#3043 = EDGE_LOOP ( 'NONE', ( #3329, #8841 ) ) ;
#3044 = CARTESIAN_POINT ( 'NONE',  ( -179.3772030532177837, 117.5545944912402661, 3.345861034185851235 ) ) ;
#3045 = CARTESIAN_POINT ( 'NONE',  ( 202.5558682508970492, 29.63341987102701580, -9.723657537314917221 ) ) ;
#3046 = ORIENTED_EDGE ( 'NONE', *, *, #1403, .F. ) ;
#3047 = DIRECTION ( 'NONE',  ( 0.000000000000000000, 0.000000000000000000, -1.000000000000000000 ) ) ;
#3048 = CARTESIAN_POINT ( 'NONE',  ( 0.000000000000000000, 0.000000000000000000, 0.000000000000000000 ) ) ;
#3049 = AXIS2_PLACEMENT_3D ( 'NONE', #2777, #9889, #7839 ) ;
#3050 = EDGE_CURVE ( 'NONE', #11465, #4254, #14521, .T. ) ;
#3051 = CARTESIAN_POINT ( 'NONE',  ( 185.1062858801516882, 25.86394065090268057, 13.00000000000000178 ) ) ;
#3052 = CARTESIAN_POINT ( 'NONE',  ( 0.000000000000000000, 6.123233995736787976E-16, -5.000000000000017764 ) ) ;
#3053 = PRODUCT_RELATED_PRODUCT_CATEGORY ( 'part', '', ( #7916 ) ) ;
#3054 = ADVANCED_FACE ( 'NONE', ( #9769 ), #906, .T. ) ;
#3055 = EDGE_LOOP ( 'NONE', ( #12716, #12912, #8, #6125 ) ) ;
#3056 = DIRECTION ( 'NONE',  ( 0.000000000000000000, 0.000000000000000000, -1.000000000000000000 ) ) ;
#3057 = CARTESIAN_POINT ( 'NONE',  ( -193.5534063424729254, 128.8169105028637205, 7.918248976830644992 ) ) ;
#3058 = CARTESIAN_POINT ( 'NONE',  ( -215.1139964504661464, 145.4140256597743814, 2.431557144026069928 ) ) ;
#3059 = EDGE_CURVE ( 'NONE', #3997, #6520, #9751, .T. ) ;
#3060 = PLANE ( 'NONE',  #12582 ) ;
#3061 = VERTEX_POINT ( 'NONE', #413 ) ;
#3063 = CARTESIAN_POINT ( 'NONE',  ( -33.09899788034579160, 48.72489408690345414, 7.600000000000002309 ) ) ;
#3062 = AXIS2_PLACEMENT_3D ( 'NONE', #5627, #1979, #706 ) ;
#3064 = VERTEX_POINT ( 'NONE', #14868 ) ;
#3065 = ORIENTED_EDGE ( 'NONE', *, *, #9925, .F. ) ;
#3066 = AXIS2_PLACEMENT_3D ( 'NONE', #4001, #8835, #9601 ) ;
#3067 = DIRECTION ( 'NONE',  ( 0.000000000000000000, -1.000000000000000000, -1.156482317317871478E-16 ) ) ;
#3068 = DIRECTION ( 'NONE',  ( -0.000000000000000000, -1.000000000000000000, -6.938893903907222067E-15 ) ) ;
#3069 = CARTESIAN_POINT ( 'NONE',  ( -169.6864937364892683, 124.2126821195596165, 9.200833310921806785 ) ) ;
#3070 = CARTESIAN_POINT ( 'NONE',  ( -216.6950415564453465, 154.8919953347533749, 2.805421358301762869 ) ) ;
#3071 = CARTESIAN_POINT ( 'NONE',  ( -110.0000000000000426, 59.53993994372674337, 10.00000000000000178 ) ) ;
#3072 = CIRCLE ( 'NONE', #9374, 1.000000000000000888 ) ;
#3073 = EDGE_CURVE ( 'NONE', #5664, #6556, #9930, .T. ) ;
#3074 = ADVANCED_FACE ( 'NONE', ( #2897 ), #4701, .T. ) ;
#3075 = CARTESIAN_POINT ( 'NONE',  ( -70.00000000000000000, 15.53993994372673626, 48.99999999999997158 ) ) ;
#3076 = AXIS2_PLACEMENT_3D ( 'NONE', #14779, #11621, #7782 ) ;
#3077 = LINE ( 'NONE', #7906, #14951 ) ;
#3078 = DIRECTION ( 'NONE',  ( -0.000000000000000000, -0.000000000000000000, 1.000000000000000000 ) ) ;
#3079 = CARTESIAN_POINT ( 'NONE',  ( -220.0166125836030915, 153.0449145671193492, -1.086335427222236527 ) ) ;
#3080 = ORIENTED_EDGE ( 'NONE', *, *, #15415, .T. ) ;
#3081 = EDGE_CURVE ( 'NONE', #831, #6280, #4689, .T. ) ;
#3082 = EDGE_LOOP ( 'NONE', ( #14976, #4117, #13374, #3753 ) ) ;
#3083 = DIRECTION ( 'NONE',  ( -0.000000000000000000, 0.000000000000000000, 1.000000000000000000 ) ) ;
#3084 = CARTESIAN_POINT ( 'NONE',  ( 2.000000000000000000, -1.587713240271472648, -2.750000000000000888 ) ) ;
#3085 = VECTOR ( 'NONE', #12143, 1000.000000000000000 ) ;
#3086 = ORIENTED_EDGE ( 'NONE', *, *, #2167, .F. ) ;
#3087 = FACE_OUTER_BOUND ( 'NONE', #6846, .T. ) ;
#3088 = DIRECTION ( 'NONE',  ( 0.000000000000000000, 0.000000000000000000, -1.000000000000000000 ) ) ;
#3089 = EDGE_CURVE ( 'NONE', #5874, #4096, #3447, .T. ) ;
#3090 = FACE_OUTER_BOUND ( 'NONE', #2207, .T. ) ;
#3091 = ORIENTED_EDGE ( 'NONE', *, *, #14050, .T. ) ;
#3092 = PRODUCT_CONTEXT ( 'NONE', #15303, 'mechanical' ) ;
#3093 = VERTEX_POINT ( 'NONE', #14646 ) ;
#3094 = CARTESIAN_POINT ( 'NONE',  ( 204.3809113867051508, 51.54681031777401756, 0.6364305089822913652 ) ) ;
#3095 = DIRECTION ( 'NONE',  ( 0.000000000000000000, -3.469446951953611033E-15, 1.000000000000000000 ) ) ;
#3096 = EDGE_LOOP ( 'NONE', ( #10306, #7313 ) ) ;
#3097 = VECTOR ( 'NONE', #7519, 1000.000000000000000 ) ;
#3098 = DIRECTION ( 'NONE',  ( 1.000000000000000000, 0.000000000000000000, 0.000000000000000000 ) ) ;
#3099 = DIRECTION ( 'NONE',  ( 1.000000000000000000, 2.751328491981765035E-32, -3.965082230804130220E-16 ) ) ;
#3100 = ORIENTED_EDGE ( 'NONE', *, *, #9245, .F. ) ;
#3101 = ORIENTED_EDGE ( 'NONE', *, *, #3843, .T. ) ;
#3102 = CARTESIAN_POINT ( 'NONE',  ( -36.49899788034579018, 48.72489408690345414, 0.000000000000000000 ) ) ;
#3103 = ORIENTED_EDGE ( 'NONE', *, *, #10488, .T. ) ;
#3104 = CARTESIAN_POINT ( 'NONE',  ( 0.000000000000000000, 0.000000000000000000, 8.000000000000007105 ) ) ;
#3105 = DIRECTION ( 'NONE',  ( 0.4873681696970814659, 0.8731965799097686221, 0.000000000000000000 ) ) ;
#3106 = EDGE_CURVE ( 'NONE', #6568, #2293, #8667, .T. ) ;
#3107 = DIRECTION ( 'NONE',  ( 0.000000000000000000, 0.000000000000000000, 1.000000000000000000 ) ) ;
#3108 = DIRECTION ( 'NONE',  ( 0.000000000000000000, 0.000000000000000000, 1.000000000000000000 ) ) ;
#3109 = CARTESIAN_POINT ( 'NONE',  ( 184.0000000000000568, 15.53993994372673981, -12.49999999999999289 ) ) ;
#3110 = PRODUCT_DEFINITION_SHAPE ( 'NONE', 'NONE',  #14036 ) ;
#3111 = LINE ( 'NONE', #13838, #2517 ) ;
#3112 = ORIENTED_EDGE ( 'NONE', *, *, #6453, .T. ) ;
#3113 = DIRECTION ( 'NONE',  ( 0.000000000000000000, 0.000000000000000000, -1.000000000000000000 ) ) ;
#3114 = CARTESIAN_POINT ( 'NONE',  ( -187.9088347589046748, 138.8287307560422903, 1.515441477536284109 ) ) ;
#3115 = LINE ( 'NONE', #4057, #3744 ) ;
#3116 = EDGE_LOOP ( 'NONE', ( #11301, #14275, #13967, #2775 ) ) ;
#3117 = CARTESIAN_POINT ( 'NONE',  ( -187.3343951027933656, 121.3449523462597313, -0.4555467707853332882 ) ) ;
#3118 = CARTESIAN_POINT ( 'NONE',  ( 192.8103048780560584, 31.45858264101640600, -1.000270116828862133 ) ) ;
#3119 = ORIENTED_EDGE ( 'NONE', *, *, #11680, .F. ) ;
#3120 = AXIS2_PLACEMENT_3D ( 'NONE', #12292, #1245, #6314 ) ;
#3121 = CARTESIAN_POINT ( 'NONE',  ( 190.5000000000000568, -181.3058001507315566, -51.45141194869120227 ) ) ;
#3122 = DIRECTION ( 'NONE',  ( 0.000000000000000000, 0.000000000000000000, 1.000000000000000000 ) ) ;
#3123 = DIRECTION ( 'NONE',  ( 1.000000000000000000, 0.000000000000000000, -0.000000000000000000 ) ) ;
#3124 = AXIS2_PLACEMENT_3D ( 'NONE', #11439, #1646, #7665 ) ;
#3125 = DIRECTION ( 'NONE',  ( -5.518327896226373923E-17, -0.9902680687415712502, -0.1391731009600586100 ) ) ;
#3126 = VERTEX_POINT ( 'NONE', #11654 ) ;
#3127 = CARTESIAN_POINT ( 'NONE',  ( 190.5000000000000853, -178.8058001507315566, 52.19066787724494816 ) ) ;
#3128 = CARTESIAN_POINT ( 'NONE',  ( -211.5791133502170283, 138.9897555992265268, 9.577123744044227394 ) ) ;
#3129 = DIRECTION ( 'NONE',  ( 0.000000000000000000, 0.000000000000000000, 1.000000000000000000 ) ) ;
#3130 = DIRECTION ( 'NONE',  ( -0.000000000000000000, 1.000000000000000000, -0.000000000000000000 ) ) ;
#3131 = ORIENTED_EDGE ( 'NONE', *, *, #9496, .F. ) ;
#3132 = EDGE_CURVE ( 'NONE', #4070, #8499, #142, .T. ) ;
#3133 = DIRECTION ( 'NONE',  ( 0.000000000000000000, -0.9902680687415713612, 0.1391731009600582492 ) ) ;
#3134 = ORIENTED_EDGE ( 'NONE', *, *, #13565, .T. ) ;
#3135 = VERTEX_POINT ( 'NONE', #9133 ) ;
#3136 = CARTESIAN_POINT ( 'NONE',  ( 177.5000000000000853, 19.53993994372674692, -17.50000000000002487 ) ) ;
#3137 = LINE ( 'NONE', #7895, #5238 ) ;
#3138 = AXIS2_PLACEMENT_3D ( 'NONE', #3457, #5827, #10723 ) ;
#3139 = EDGE_CURVE ( 'NONE', #9730, #5113, #11517, .T. ) ;
#3140 = DIRECTION ( 'NONE',  ( 1.000000000000000000, 0.000000000000000000, 0.000000000000000000 ) ) ;
#3141 = CARTESIAN_POINT ( 'NONE',  ( -172.7942878933874908, 118.6445810460862873, 8.630634598295349846 ) ) ;
#3142 = CARTESIAN_POINT ( 'NONE',  ( -220.5827524467639762, 152.0305861332991526, -2.167411311894018144 ) ) ;
#3143 = DIRECTION ( 'NONE',  ( -0.000000000000000000, 1.000000000000000000, -0.000000000000000000 ) ) ;
#3144 = CARTESIAN_POINT ( 'NONE',  ( -110.0000000000000426, 22.53993994372673981, 13.00000000000000178 ) ) ;
#3145 = DIRECTION ( 'NONE',  ( 0.000000000000000000, -0.4999999999999996669, 0.8660254037844388186 ) ) ;
#3146 = CARTESIAN_POINT ( 'NONE',  ( -150.4086188282879277, 107.2728346664360259, 5.000000000000000000 ) ) ;
#3147 = AXIS2_PLACEMENT_3D ( 'NONE', #8822, #2824, #2665 ) ;
#3148 = CARTESIAN_POINT ( 'NONE',  ( -222.6481022377596446, 148.3301877775025162, -2.885485496913823056 ) ) ;
#3149 = ORIENTED_EDGE ( 'NONE', *, *, #3532, .T. ) ;
#3150 =( LENGTH_UNIT ( ) NAMED_UNIT ( * ) SI_UNIT ( .MILLI., .METRE. ) );
#3151 = ORIENTED_EDGE ( 'NONE', *, *, #2188, .F. ) ;
#3152 = DIRECTION ( 'NONE',  ( 0.000000000000000000, 0.000000000000000000, -1.000000000000000000 ) ) ;
#3153 = CARTESIAN_POINT ( 'NONE',  ( 178.0000000000000853, -179.8058001507315566, 52.49999999999997868 ) ) ;
#3154 = EDGE_CURVE ( 'NONE', #15074, #14924, #8737, .T. ) ;
#3155 = EDGE_CURVE ( 'NONE', #8328, #10124, #9208, .T. ) ;
#3156 = ORIENTED_EDGE ( 'NONE', *, *, #5172, .T. ) ;
#3157 = ADVANCED_FACE ( 'NONE', ( #12738 ), #2162, .T. ) ;
#3158 = DIRECTION ( 'NONE',  ( -3.965082230804130220E-16, 4.956352788505162775E-17, -1.000000000000000000 ) ) ;
#3159 = LINE ( 'NONE', #4413, #4049 ) ;
#3160 = CIRCLE ( 'NONE', #5179, 1.700000000000000178 ) ;
#3161 = CYLINDRICAL_SURFACE ( 'NONE', #15186, 1.000000000000000888 ) ;
#3162 = ORIENTED_EDGE ( 'NONE', *, *, #11620, .F. ) ;
#3163 = ITEM_DEFINED_TRANSFORMATION ( 'NONE', 'NONE', #4753,  #12337 ) ;
#3164 = EDGE_LOOP ( 'NONE', ( #4569, #10359, #9499 ) ) ;
#3165 = CARTESIAN_POINT ( 'NONE',  ( 198.3905366428873549, 52.61667164843417765, -5.260075093946414704 ) ) ;
#3166 = ORIENTED_EDGE ( 'NONE', *, *, #6294, .F. ) ;
#3167 = DIRECTION ( 'NONE',  ( -0.000000000000000000, 0.000000000000000000, -1.000000000000000000 ) ) ;
#3168 = EDGE_CURVE ( 'NONE', #815, #12081, #11568, .T. ) ;
#3169 = AXIS2_PLACEMENT_3D ( 'NONE', #11001, #12406, #14766 ) ;
#3170 = DIRECTION ( 'NONE',  ( -0.000000000000000000, 1.000000000000000000, -0.000000000000000000 ) ) ;
#3171 = ORIENTED_EDGE ( 'NONE', *, *, #1484, .T. ) ;
#3172 = ORIENTED_EDGE ( 'NONE', *, *, #5741, .T. ) ;
#3173 = DIRECTION ( 'NONE',  ( -0.7071067811864983899, 8.659560562354331352E-17, 0.7071067811865966446 ) ) ;
#3174 = AXIS2_PLACEMENT_3D ( 'NONE', #4450, #5576, #14006 ) ;
#3175 = ORIENTED_EDGE ( 'NONE', *, *, #10058, .T. ) ;
#3176 = CARTESIAN_POINT ( 'NONE',  ( 208.8162124854775357, 42.04914431719598156, -1.433821094984975009 ) ) ;
#3177 = DIRECTION ( 'NONE',  ( 0.000000000000000000, -1.000000000000000000, -6.938893903907227145E-17 ) ) ;
#3178 = CARTESIAN_POINT ( 'NONE',  ( 178.0000000000000853, -179.8058001507315566, 84.88378295107887084 ) ) ;
#3179 = CYLINDRICAL_SURFACE ( 'NONE', #13769, 1.499999999999994449 ) ;
#3180 = CYLINDRICAL_SURFACE ( 'NONE', #7074, 5.000000000000004441 ) ;
#3181 = AXIS2_PLACEMENT_3D ( 'NONE', #8514, #6140, #4789 ) ;
#3182 = CARTESIAN_POINT ( 'NONE',  ( 224.0000000000000853, 59.53993994372674337, 25.00000000000000000 ) ) ;
#3183 = EDGE_CURVE ( 'NONE', #10985, #5154, #580, .T. ) ;
#3184 = EDGE_CURVE ( 'NONE', #5606, #3200, #528, .T. ) ;
#3185 = ORIENTED_EDGE ( 'NONE', *, *, #4300, .T. ) ;
#3186 = CARTESIAN_POINT ( 'NONE',  ( 184.0000000000000568, -201.3058001507315566, -42.95141194869119516 ) ) ;
#3187 = EDGE_CURVE ( 'NONE', #11085, #9186, #12579, .T. ) ;
#3188 = CARTESIAN_POINT ( 'NONE',  ( -175.7692568323954845, 129.7291524912800185, -2.973479603620230893 ) ) ;
#3189 = DIRECTION ( 'NONE',  ( -0.9429519417310716634, 0.3294944882152614496, 0.04769714688914629408 ) ) ;
#3190 = ORIENTED_EDGE ( 'NONE', *, *, #10504, .T. ) ;
#3191 = CARTESIAN_POINT ( 'NONE',  ( -175.8505196906716890, 123.8775902107358036, -5.297343846388533173 ) ) ;
#3192 = CARTESIAN_POINT ( 'NONE',  ( 198.5781842723177704, 29.07471546161169229, -6.884323831650920766 ) ) ;
#3193 = ORIENTED_EDGE ( 'NONE', *, *, #13553, .T. ) ;
#3194 = DIRECTION ( 'NONE',  ( -0.000000000000000000, 1.000000000000000000, 0.000000000000000000 ) ) ;
#3195 = CARTESIAN_POINT ( 'NONE',  ( 0.1709786460671990638, -1.329147683181058692, 2.749999999999999556 ) ) ;
#3196 = CARTESIAN_POINT ( 'NONE',  ( 177.5000000000000853, 15.53993994372673626, 52.49999999999997868 ) ) ;
#3197 = ORIENTED_EDGE ( 'NONE', *, *, #13242, .T. ) ;
#3198 = DIRECTION ( 'NONE',  ( 1.000000000000000000, -2.751328491981765035E-32, 3.965082230804130220E-16 ) ) ;
#3199 = EDGE_CURVE ( 'NONE', #15193, #6271, #15179, .T. ) ;
#3200 = VERTEX_POINT ( 'NONE', #813 ) ;
#3201 = FACE_OUTER_BOUND ( 'NONE', #2446, .T. ) ;
#3202 = CARTESIAN_POINT ( 'NONE',  ( -220.6842914767384229, 151.8486630221608209, 9.556866313350491637 ) ) ;
#3203 = CARTESIAN_POINT ( 'NONE',  ( 50.57199999999998852, 0.000000000000000000, 0.000000000000000000 ) ) ;
#3204 = DIRECTION ( 'NONE',  ( -0.000000000000000000, 1.156482317317871478E-16, -1.000000000000000000 ) ) ;
#3205 = ORIENTED_EDGE ( 'NONE', *, *, #2553, .F. ) ;
#3206 = DIRECTION ( 'NONE',  ( -1.000000000000000000, 0.000000000000000000, 0.000000000000000000 ) ) ;
#3207 = ORIENTED_EDGE ( 'NONE', *, *, #3762, .F. ) ;
#3208 = ORIENTED_EDGE ( 'NONE', *, *, #12766, .T. ) ;
#3209 = CARTESIAN_POINT ( 'NONE',  ( -222.5463326935617658, 144.4088500683630514, 2.431557144026069928 ) ) ;
#3210 = LINE ( 'NONE', #6631, #6763 ) ;
#3211 = ADVANCED_FACE ( 'NONE', ( #2005 ), #13853, .F. ) ;
#3212 = FACE_BOUND ( 'NONE', #10839, .T. ) ;
#3213 = CARTESIAN_POINT ( 'NONE',  ( -173.5807750188128296, 117.2354659032339299, 6.976364879781497663 ) ) ;
#3214 = CARTESIAN_POINT ( 'NONE',  ( -222.6481022377693932, 148.3301877774849800, -2.885485496940157990 ) ) ;
#3215 = EDGE_CURVE ( 'NONE', #10303, #5951, #13758, .T. ) ;
#3216 = DIRECTION ( 'NONE',  ( -1.000000000000000000, 0.000000000000000000, 0.000000000000000000 ) ) ;
#3217 =( REPRESENTATION_RELATIONSHIP ('NONE','NONE', #3298, #5419 ) REPRESENTATION_RELATIONSHIP_WITH_TRANSFORMATION ( #3163 )SHAPE_REPRESENTATION_RELATIONSHIP( ) );
#3218 = DIRECTION ( 'NONE',  ( 0.000000000000000000, 1.000000000000000000, 0.000000000000000000 ) ) ;
#3219 = CARTESIAN_POINT ( 'NONE',  ( 122.5806775638430253, 45.00321902537314145, 5.000000000000000000 ) ) ;
#3220 = FACE_OUTER_BOUND ( 'NONE', #10906, .T. ) ;
#3221 = EDGE_CURVE ( 'NONE', #13828, #11543, #6612, .T. ) ;
#3222 = CIRCLE ( 'NONE', #7529, 0.5000000000000004441 ) ;
#3223 = CARTESIAN_POINT ( 'NONE',  ( -224.4522725256417743, 145.0977334997998014, 0.6248101478054410851 ) ) ;
#3224 = ORIENTED_EDGE ( 'NONE', *, *, #938, .T. ) ;
#3225 = AXIS2_PLACEMENT_3D ( 'NONE', #13000, #14185, #5466 ) ;
#3226 = EDGE_LOOP ( 'NONE', ( #7677, #1250, #9326, #7247 ) ) ;
#3227 = CARTESIAN_POINT ( 'NONE',  ( 172.0899380277727744, 70.88000906936352408, -0.9107274384406883749 ) ) ;
#3228 = CARTESIAN_POINT ( 'NONE',  ( 5.799999999999999822, 7.999999999999979572, 0.000000000000000000 ) ) ;
#3229 = ORIENTED_EDGE ( 'NONE', *, *, #6397, .T. ) ;
#3230 = LINE ( 'NONE', #14119, #2375 ) ;
#3231 = CARTESIAN_POINT ( 'NONE',  ( 169.0293059057019889, 61.25683321636181233, 9.975000000000001421 ) ) ;
#3232 = PRODUCT_DEFINITION_SHAPE ( 'NONE', 'NONE',  #15380 ) ;
#3233 = CIRCLE ( 'NONE', #8843, 0.5000000000000004441 ) ;
#3234 = DIRECTION ( 'NONE',  ( 0.000000000000000000, 0.1391731009600660485, -0.9902680687415702510 ) ) ;
#3235 = EDGE_LOOP ( 'NONE', ( #1919, #2596 ) ) ;
#3236 = ORIENTED_EDGE ( 'NONE', *, *, #1603, .T. ) ;
#3237 = ADVANCED_FACE ( 'NONE', ( #9282 ), #8114, .T. ) ;
#3238 = CARTESIAN_POINT ( 'NONE',  ( 207.2638851143210275, 31.35908548908414417, -0.3703513705075706097 ) ) ;
#3240 = ADVANCED_FACE ( 'NONE', ( #14079 ), #6919, .F. ) ;
#3239 = ADVANCED_FACE ( 'NONE', ( #6691 ), #10740, .T. ) ;
#3241 = FACE_BOUND ( 'NONE', #13785, .T. ) ;
#3242 = EDGE_LOOP ( 'NONE', ( #3667, #6099, #3351, #12849 ) ) ;
#3243 = DIRECTION ( 'NONE',  ( 0.000000000000000000, 0.000000000000000000, 1.000000000000000000 ) ) ;
#3244 = DIRECTION ( 'NONE',  ( 0.8731965799097684000, -0.4873681696970819655, -0.000000000000000000 ) ) ;
#3245 = VERTEX_POINT ( 'NONE', #7235 ) ;
#3246 = ADVANCED_FACE ( 'NONE', ( #15412, #14235, #3659, #4686, #9438, #10860, #12031 ), #4532, .T. ) ;
#3247 = ORIENTED_EDGE ( 'NONE', *, *, #1753, .T. ) ;
#3248 = DIRECTION ( 'NONE',  ( 1.000000000000000000, 0.000000000000000000, 0.000000000000000000 ) ) ;
#3249 = CARTESIAN_POINT ( 'NONE',  ( -223.5985612785965486, 142.0411530078025635, 1.742203648027802254 ) ) ;
#3250 = AXIS2_PLACEMENT_3D ( 'NONE', #4534, #15256, #2006 ) ;
#3251 = AXIS2_PLACEMENT_3D ( 'NONE', #7788, #407, #5244 ) ;
#3252 = ORIENTED_EDGE ( 'NONE', *, *, #9048, .F. ) ;
#3253 = CARTESIAN_POINT ( 'NONE',  ( -76.50000000000004263, -179.8058001507315566, 65.31842631998698323 ) ) ;
#3254 = DIRECTION ( 'NONE',  ( 1.000000000000000000, 0.000000000000000000, 0.000000000000000000 ) ) ;
#3255 = DIRECTION ( 'NONE',  ( 0.000000000000000000, 0.5000000000000019984, 0.8660254037844375974 ) ) ;
#3256 = CARTESIAN_POINT ( 'NONE',  ( 176.0543059057019661, 61.25683321636181233, 10.00000000000000178 ) ) ;
#3257 = DIRECTION ( 'NONE',  ( 1.000000000000000000, 0.000000000000000000, 0.000000000000000000 ) ) ;
#3258 = VECTOR ( 'NONE', #4124, 1000.000000000000114 ) ;
#3259 = VECTOR ( 'NONE', #4688, 1000.000000000000000 ) ;
#3260 = AXIS2_PLACEMENT_3D ( 'NONE', #8787, #7927, #7850 ) ;
#3261 = EDGE_CURVE ( 'NONE', #14091, #858, #3588, .T. ) ;
#3262 = DIRECTION ( 'NONE',  ( 0.000000000000000000, 0.000000000000000000, -1.000000000000000000 ) ) ;
#3263 = VERTEX_POINT ( 'NONE', #5881 ) ;
#3264 = CARTESIAN_POINT ( 'NONE',  ( 172.5293059057019889, 61.25683321636181233, 10.00000000000000178 ) ) ;
#3265 = CARTESIAN_POINT ( 'NONE',  ( -204.1471980322648960, 142.4963817258166614, -4.640918829492428621 ) ) ;
#3266 = DIRECTION ( 'NONE',  ( 0.000000000000000000, -1.000000000000000000, 0.000000000000000000 ) ) ;
#3267 = CIRCLE ( 'NONE', #12088, 1.499999999999994449 ) ;
#3268 = ORIENTED_EDGE ( 'NONE', *, *, #13753, .T. ) ;
#3269 = CARTESIAN_POINT ( 'NONE',  ( -194.2672495621651478, 127.5518908598051127, -0.4555467707853320669 ) ) ;
#3270 = CARTESIAN_POINT ( 'NONE',  ( 207.3157014670556748, 31.37515976295564357, -6.367693553816072161 ) ) ;
#3271 = AXIS2_PLACEMENT_3D ( 'NONE', #4361, #1683, #12650 ) ;
#3272 = EDGE_CURVE ( 'NONE', #2490, #1161, #9511, .T. ) ;
#3273 = ORIENTED_EDGE ( 'NONE', *, *, #36, .F. ) ;
#3274 = VECTOR ( 'NONE', #1642, 1000.000000000000000 ) ;
#3275 = AXIS2_PLACEMENT_3D ( 'NONE', #13025, #14216, #6677 ) ;
#3276 = LINE ( 'NONE', #11800, #15341 ) ;
#3277 = DIRECTION ( 'NONE',  ( 0.8731965799097682890, -0.4873681696970819099, 0.000000000000000000 ) ) ;
#3278 = CARTESIAN_POINT ( 'NONE',  ( -63.50000000000002842, 16.03993994372673626, 52.49999999999997868 ) ) ;
#3279 = EDGE_CURVE ( 'NONE', #435, #9262, #14, .T. ) ;
#3280 = VECTOR ( 'NONE', #2497, 1000.000000000000000 ) ;
#3281 = ORIENTED_EDGE ( 'NONE', *, *, #2039, .F. ) ;
#3282 = AXIS2_PLACEMENT_3D ( 'NONE', #3576, #4757, #12965 ) ;
#3283 = DIRECTION ( 'NONE',  ( 1.000000000000000000, 0.000000000000000000, 0.000000000000000000 ) ) ;
#3284 = CIRCLE ( 'NONE', #14873, 1.500000000000001332 ) ;
#3285 = DIRECTION ( 'NONE',  ( 0.000000000000000000, 0.1391731009600591096, -0.9902680687415711391 ) ) ;
#3286 = EDGE_LOOP ( 'NONE', ( #3980, #9995, #684, #12442 ) ) ;
#3287 = FACE_OUTER_BOUND ( 'NONE', #14716, .T. ) ;
#3288 = CARTESIAN_POINT ( 'NONE',  ( -210.0240857098682454, 141.7683007401625446, 10.16010209732750624 ) ) ;
#3289 = DIRECTION ( 'NONE',  ( -1.000000000000000000, 0.000000000000000000, 0.000000000000000000 ) ) ;
#3290 = DIRECTION ( 'NONE',  ( -1.000000000000000000, 0.000000000000000000, 0.000000000000000000 ) ) ;
#3291 = ORIENTED_EDGE ( 'NONE', *, *, #5066, .F. ) ;
#3292 = CARTESIAN_POINT ( 'NONE',  ( -76.00000000000001421, 16.03993994372673981, -3.075184203610571654 ) ) ;
#3293 = ORIENTED_EDGE ( 'NONE', *, *, #12381, .T. ) ;
#3294 = ORIENTED_EDGE ( 'NONE', *, *, #2591, .F. ) ;
#3295 = AXIS2_PLACEMENT_3D ( 'NONE', #76, #10841, #12238 ) ;
#3296 = CARTESIAN_POINT ( 'NONE',  ( 190.0000000000000853, -179.8058001507315566, 52.19066787724494816 ) ) ;
#3297 = CARTESIAN_POINT ( 'NONE',  ( 190.0000000000000568, -178.8058001507315566, 52.69066787724494816 ) ) ;
#3298 = SHAPE_REPRESENTATION ( 'MAS-307', ( #11066, #2228, #12315, #8056, #9804, #4753, #15077, #1205, #10823, #15585, #10555, #14068, #4491, #15319, #8048, #3491 ), #13059 ) ;
#3299 = CIRCLE ( 'NONE', #5312, 0.4999999999999996114 ) ;
#3300 = DIRECTION ( 'NONE',  ( 1.000000000000000000, 0.000000000000000000, -0.000000000000000000 ) ) ;
#3301 = CARTESIAN_POINT ( 'NONE',  ( -174.0007056342363683, 116.4830942877151756, 5.347843459918403930 ) ) ;
#3302 = CARTESIAN_POINT ( 'NONE',  ( -224.7501301915791601, 144.5640747355008671, -2.630842070996033399 ) ) ;
#3303 = EDGE_CURVE ( 'NONE', #11700, #13949, #9738, .T. ) ;
#3304 = DIRECTION ( 'NONE',  ( -0.000000000000000000, -0.000000000000000000, 1.000000000000000000 ) ) ;
#3305 = PLANE ( 'NONE',  #11687 ) ;
#3306 = CIRCLE ( 'NONE', #12125, 1.699999999999993072 ) ;
#3307 = DIRECTION ( 'NONE',  ( 0.000000000000000000, 0.000000000000000000, 1.000000000000000000 ) ) ;
#3308 = VECTOR ( 'NONE', #10953, 1000.000000000000114 ) ;
#3309 = DIRECTION ( 'NONE',  ( -0.000000000000000000, 1.000000000000000000, -0.000000000000000000 ) ) ;
#3310 = CARTESIAN_POINT ( 'NONE',  ( 126.0806775638430253, 45.00321902537314145, 9.975000000000001421 ) ) ;
#3311 = ORIENTED_EDGE ( 'NONE', *, *, #4911, .T. ) ;
#3312 = ORIENTED_EDGE ( 'NONE', *, *, #9621, .T. ) ;
#3313 = CARTESIAN_POINT ( 'NONE',  ( 175.9483885134608272, -179.3058001507315566, 52.76585208085545275 ) ) ;
#3314 = VERTEX_POINT ( 'NONE', #10620 ) ;
#3315 = DIRECTION ( 'NONE',  ( -0.000000000000000000, -0.000000000000000000, 1.000000000000000000 ) ) ;
#3316 = CARTESIAN_POINT ( 'NONE',  ( -135.4906327255880569, 109.5619692454514791, 2.431557144026069928 ) ) ;
#3317 = CIRCLE ( 'NONE', #12134, 0.4999999999999998890 ) ;
#3318 = ADVANCED_FACE ( 'NONE', ( #1056 ), #15561, .F. ) ;
#3319 = VECTOR ( 'NONE', #6126, 1000.000000000000000 ) ;
#3320 = VERTEX_POINT ( 'NONE', #11801 ) ;
#3321 = ORIENTED_EDGE ( 'NONE', *, *, #705, .T. ) ;
#3322 = CARTESIAN_POINT ( 'NONE',  ( 211.8657363685815653, 42.56416725473636831, -9.010781945348840694 ) ) ;
#3323 = LINE ( 'NONE', #12943, #9386 ) ;
#3324 = VERTEX_POINT ( 'NONE', #5955 ) ;
#3325 = DIRECTION ( 'NONE',  ( 0.000000000000000000, 0.5000000000000011102, -0.8660254037844380415 ) ) ;
#3326 = CIRCLE ( 'NONE', #7126, 1.499999999999994449 ) ;
#3327 = CARTESIAN_POINT ( 'NONE',  ( -63.50000000000002842, -181.3058001507315566, -51.45141194869119516 ) ) ;
#3328 = CARTESIAN_POINT ( 'NONE',  ( -224.6003768274171080, 144.8323813947157817, 2.186315064719954737 ) ) ;
#3329 = ORIENTED_EDGE ( 'NONE', *, *, #11650, .T. ) ;
#3330 = ORIENTED_EDGE ( 'NONE', *, *, #6997, .T. ) ;
#3331 = DIRECTION ( 'NONE',  ( 0.7071067811865965336, 0.000000000000000000, 0.7071067811864985009 ) ) ;
#3332 = EDGE_CURVE ( 'NONE', #13022, #11585, #2421, .T. ) ;
#3333 = DIRECTION ( 'NONE',  ( 1.000000000000000000, 0.000000000000000000, 0.000000000000000000 ) ) ;
#3334 = ORIENTED_EDGE ( 'NONE', *, *, #1545, .T. ) ;
#3335 = CARTESIAN_POINT ( 'NONE',  ( -152.4086188282879277, 107.2728346664360259, 9.411501811869209533 ) ) ;
#3336 = LINE ( 'NONE', #12718, #5801 ) ;
#3337 = EDGE_CURVE ( 'NONE', #10460, #207, #1468, .T. ) ;
#3338 = EDGE_CURVE ( 'NONE', #7982, #85, #4427, .T. ) ;
#3339 = DIRECTION ( 'NONE',  ( -1.000000000000000000, 0.000000000000000000, 0.000000000000000000 ) ) ;
#3340 = AXIS2_PLACEMENT_3D ( 'NONE', #11092, #5089, #13367 ) ;
#3341 = ADVANCED_FACE ( 'NONE', ( #9360 ), #13124, .T. ) ;
#3342 = CLOSED_SHELL ( 'NONE', ( #11213, #3618, #12672, #6536, #14105, #15185, #8759, #4502, #15099, #14743, #14333, #5186, #5083, #2641, #12395, #1116, #5218, #9138, #8161, #14456, #4398, #5956, #2864, #6360, #13173, #2707, #12566, #4895, #12029, #15184, #13156, #10949, #11482, #5715, #9934, #7666, #10564, #417, #9754, #11415, #4597, #5464, #14352, #1417, #14875, #6632, #3353, #2281, #3341, #3024, #1344, #13864, #3074, #3157, #3500, #14125, #3632, #12248, #10826, #8770, #7606, #11467, #8849, #15064, #6651, #10683, #8129, #8943, #3421, #881, #4036, #9521, #3812, #11551, #7011, #15221 ) ) ;
#3343 = CARTESIAN_POINT ( 'NONE',  ( 177.5000000000000853, 17.53993994372674692, -17.50000000000002487 ) ) ;
#3344 = VERTEX_POINT ( 'NONE', #4765 ) ;
#3345 = CARTESIAN_POINT ( 'NONE',  ( 190.5000000000000853, -178.8058001507315566, 65.31842631998698323 ) ) ;
#3346 = LINE ( 'NONE', #8330, #13366 ) ;
#3347 = CARTESIAN_POINT ( 'NONE',  ( 184.0000000000000568, 19.53993994372673626, 45.99999999999998579 ) ) ;
#3348 = ORIENTED_EDGE ( 'NONE', *, *, #11478, .F. ) ;
#3349 = CARTESIAN_POINT ( 'NONE',  ( -192.4489746382803048, 130.7761537121523361, -4.642206099735005864 ) ) ;
#3350 = CARTESIAN_POINT ( 'NONE',  ( 198.5455061167297117, 29.08454594588317477, -3.885748181069116569 ) ) ;
#3351 = ORIENTED_EDGE ( 'NONE', *, *, #6517, .T. ) ;
#3352 = VECTOR ( 'NONE', #5067, 1000.000000000000000 ) ;
#3353 = ADVANCED_FACE ( 'NONE', ( #3356 ), #9672, .T. ) ;
#3354 = EDGE_CURVE ( 'NONE', #7696, #5990, #10233, .T. ) ;
#3355 = CARTESIAN_POINT ( 'NONE',  ( 185.1062858801516597, 25.86394065090268057, 13.00000000000000178 ) ) ;
#3356 = FACE_OUTER_BOUND ( 'NONE', #4362, .T. ) ;
#3357 = EDGE_CURVE ( 'NONE', #12329, #15368, #3013, .T. ) ;
#3358 = AXIS2_PLACEMENT_3D ( 'NONE', #4025, #688, #1810 ) ;
#3359 = CARTESIAN_POINT ( 'NONE',  ( -150.4086188282879277, 107.2728346664360259, -4.856732557889654522 ) ) ;
#3360 = ORIENTED_EDGE ( 'NONE', *, *, #3184, .T. ) ;
#3361 = CARTESIAN_POINT ( 'NONE',  ( 208.8213467238098247, 41.99652926550911758, -5.863399402755005596 ) ) ;
#3362 = ORIENTED_EDGE ( 'NONE', *, *, #8963, .F. ) ;
#3363 = LINE ( 'NONE', #98, #2657 ) ;
#3364 = AXIS2_PLACEMENT_3D ( 'NONE', #3610, #10802, #9534 ) ;
#3365 = CARTESIAN_POINT ( 'NONE',  ( -176.6594047394515314, 116.7136007993067324, 3.281269053145625225 ) ) ;
#3366 = CARTESIAN_POINT ( 'NONE',  ( 165.1224552381025887, 111.1124422548786299, 5.000000000000000000 ) ) ;
#3367 = DIRECTION ( 'NONE',  ( -1.000000000000000000, 0.000000000000000000, 0.000000000000000000 ) ) ;
#3368 = PLANE ( 'NONE',  #11630 ) ;
#3369 = EDGE_CURVE ( 'NONE', #2394, #14442, #15255, .T. ) ;
#3370 = ORIENTED_EDGE ( 'NONE', *, *, #8761, .F. ) ;
#3371 = EDGE_LOOP ( 'NONE', ( #1596, #4260, #5476, #14353 ) ) ;
#3372 = DIRECTION ( 'NONE',  ( -0.000000000000000000, -0.000000000000000000, 1.000000000000000000 ) ) ;
#3373 = CARTESIAN_POINT ( 'NONE',  ( 114.0000000000000568, 62.13993994372673768, 15.00000000000035172 ) ) ;
#3374 = CARTESIAN_POINT ( 'NONE',  ( -64.00000000000002842, 15.03993994372673804, 37.57518420361041933 ) ) ;
#3375 = DIRECTION ( 'NONE',  ( -0.000000000000000000, 1.000000000000000000, 8.673617379884035472E-17 ) ) ;
#3376 = CARTESIAN_POINT ( 'NONE',  ( -223.7005213066090334, 146.4446138137323317, -1.719282361323794861 ) ) ;
#3377 = CIRCLE ( 'NONE', #15457, 1.700000000000007061 ) ;
#3378 = DIRECTION ( 'NONE',  ( 3.965082230804130220E-16, -4.956352788505162775E-17, 1.000000000000000000 ) ) ;
#3379 = AXIS2_PLACEMENT_3D ( 'NONE', #4951, #15510, #8442 ) ;
#3380 = DIRECTION ( 'NONE',  ( 0.000000000000000000, 0.000000000000000000, -1.000000000000000000 ) ) ;
#3381 = DIRECTION ( 'NONE',  ( -0.000000000000000000, -0.000000000000000000, 1.000000000000000000 ) ) ;
#3382 = FACE_OUTER_BOUND ( 'NONE', #12254, .T. ) ;
#3383 = EDGE_CURVE ( 'NONE', #4243, #61, #11087, .T. ) ;
#3384 = CARTESIAN_POINT ( 'NONE',  ( -70.00000000000000000, 15.53993994372673981, -10.99999999999999645 ) ) ;
#3385 = LINE ( 'NONE', #14109, #4587 ) ;
#3386 = ORIENTED_EDGE ( 'NONE', *, *, #2682, .F. ) ;
#3387 = SHAPE_REPRESENTATION ( 'hex bolt gradeab_iso_ISO 4014 - M10 x 45 x 26-N', ( #12337 ), #10810 ) ;
#3388 = SHAPE_REPRESENTATION_RELATIONSHIP ( 'NONE' , 'NONE' ,  #8648, #15417 ) ;
#3389 = VERTEX_POINT ( 'NONE', #6273 ) ;
#3390 = DIRECTION ( 'NONE',  ( -0.000000000000000000, 6.938893903907222067E-15, -1.000000000000000000 ) ) ;
#3391 = LINE ( 'NONE', #5837, #8620 ) ;
#3393 = CARTESIAN_POINT ( 'NONE',  ( 0.000000000000000000, -6.928203230275514990, 4.000000000000058620 ) ) ;
#3392 = VECTOR ( 'NONE', #4174, 1000.000000000000000 ) ;
#3394 = CARTESIAN_POINT ( 'NONE',  ( -172.4561068142338058, 130.1936157287141498, 2.500000000515479215 ) ) ;
#3395 = DIRECTION ( 'NONE',  ( 0.000000000000000000, 0.000000000000000000, 1.000000000000000000 ) ) ;
#3396 = ORIENTED_EDGE ( 'NONE', *, *, #10958, .T. ) ;
#3397 = VECTOR ( 'NONE', #12363, 1000.000000000000000 ) ;
#3398 = EDGE_CURVE ( 'NONE', #3061, #15478, #3899, .T. ) ;
#3399 = ORIENTED_EDGE ( 'NONE', *, *, #10257, .T. ) ;
#3400 = CARTESIAN_POINT ( 'NONE',  ( 192.9750851430037528, 31.35397111148814631, -7.136603044727629630 ) ) ;
#3401 = DIRECTION ( 'NONE',  ( 0.000000000000000000, 0.000000000000000000, 1.000000000000000000 ) ) ;
#3402 = EDGE_LOOP ( 'NONE', ( #9415, #8983, #583, #2926 ) ) ;
#3403 = CYLINDRICAL_SURFACE ( 'NONE', #3429, 1.699999999999991518 ) ;
#3404 = DIRECTION ( 'NONE',  ( 0.000000000000000000, 1.000000000000000000, 6.938893903907227145E-17 ) ) ;
#3405 = DIRECTION ( 'NONE',  ( -0.000000000000000000, -0.000000000000000000, 1.000000000000000000 ) ) ;
#3406 = ORIENTED_EDGE ( 'NONE', *, *, #6142, .F. ) ;
#3407 = ORIENTED_EDGE ( 'NONE', *, *, #15254, .T. ) ;
#3408 = CARTESIAN_POINT ( 'NONE',  ( -76.00000000000001421, -178.8058001507315566, 53.19066787724494816 ) ) ;
#3409 = LINE ( 'NONE', #13021, #261 ) ;
#3410 = AXIS2_PLACEMENT_3D ( 'NONE', #14547, #8891, #12496 ) ;
#3411 = ORIENTED_EDGE ( 'NONE', *, *, #3721, .F. ) ;
#3412 = CARTESIAN_POINT ( 'NONE',  ( 120.8806775638430224, 45.00321902537314145, 5.000000000000000000 ) ) ;
#3413 = EDGE_CURVE ( 'NONE', #234, #10340, #1436, .T. ) ;
#3414 = DIRECTION ( 'NONE',  ( -0.000000000000000000, 1.000000000000000000, -0.000000000000000000 ) ) ;
#3415 = CIRCLE ( 'NONE', #2666, 1.699999999999993072 ) ;
#3416 = ORIENTED_EDGE ( 'NONE', *, *, #10935, .T. ) ;
#3417 = CARTESIAN_POINT ( 'NONE',  ( -63.50000000000002842, 15.10952649420676863, 9.557440204760681013 ) ) ;
#3418 = ORIENTED_EDGE ( 'NONE', *, *, #14970, .F. ) ;
#3419 = TOROIDAL_SURFACE ( 'NONE', #5444, 1.000000000000000000, 0.5000000000000000000 ) ;
#3420 = DIRECTION ( 'NONE',  ( -1.000000000000000000, 0.000000000000000000, 0.000000000000000000 ) ) ;
#3421 = ADVANCED_FACE ( 'NONE', ( #12415 ), #14755, .T. ) ;
#3422 = DIRECTION ( 'NONE',  ( 0.000000000000000000, 0.9953381730041138686, 0.09644646888731951695 ) ) ;
#3423 = PLANE ( 'NONE',  #972 ) ;
#3424 = ORIENTED_EDGE ( 'NONE', *, *, #7515, .F. ) ;
#3425 = CARTESIAN_POINT ( 'NONE',  ( -212.8881127827856687, 136.6510672405775892, -2.964974570226852624 ) ) ;
#3426 = UNCERTAINTY_MEASURE_WITH_UNIT (LENGTH_MEASURE( 1.000000000000000082E-05 ), #15053, 'distance_accuracy_value', 'NONE');
#3427 = CARTESIAN_POINT ( 'NONE',  ( 208.7906731791537425, 42.14840350977979710, -9.001400940668622397 ) ) ;
#3428 = ORIENTED_EDGE ( 'NONE', *, *, #5673, .F. ) ;
#3429 = AXIS2_PLACEMENT_3D ( 'NONE', #4736, #1024, #9560 ) ;
#3430 = DIRECTION ( 'NONE',  ( 1.000000000000000000, 0.000000000000000000, 0.000000000000000000 ) ) ;
#3431 = DIRECTION ( 'NONE',  ( -5.518327896226373923E-17, 0.9902680687415712502, 0.1391731009600586100 ) ) ;
#3432 = FACE_OUTER_BOUND ( 'NONE', #12476, .T. ) ;
#3433 = B_SPLINE_CURVE_WITH_KNOTS ( 'NONE', 3,
 ( #15134, #15051, #5364, #4166, #6486, #4406, #5446, #766, #9235, #3079, #7908, #2998, #6719, #10183, #11522, #13964, #11283, #11442, #5525, #4095, #4325, #10260, #8928, #9165, #3148, #13885, #7981, #12768, #1725, #5604, #13722, #10416, #15211, #14033, #2925, #7748, #3223, #8060, #1649, #443 ),
 .UNSPECIFIED., .F., .F.,
 ( 4, 2, 2, 2, 2, 2, 2, 2, 2, 2, 2, 2, 2, 2, 2, 2, 2, 2, 2, 4 ),
 ( 0.01642013739010526191, 0.01748450029317128937, 0.01854886319623732030, 0.01961322609930334776, 0.02067758900236937869, 0.02120977045390238375, 0.02174195190543538880, 0.02280631480850148565, 0.02387067771156758250, 0.02493504061463367588, 0.02599940351769977273, 0.02653158496923285758, 0.02706376642076593897, 0.02812812932383207051, 0.02919249222689820206, 0.03025685512996433013, 0.03132121803303045821, 0.03185339948456353265, 0.03238558093609660016, 0.03344994383916276293 ),
 .UNSPECIFIED. ) ;
#3434 = ORIENTED_EDGE ( 'NONE', *, *, #4211, .F. ) ;
#3435 = CARTESIAN_POINT ( 'NONE',  ( -36.49899788034579018, 48.72489408690345414, 5.000000000000000000 ) ) ;
#3436 = CARTESIAN_POINT ( 'NONE',  ( 208.8051451104704768, 39.65587490144260840, -4.559632177755815086 ) ) ;
#3437 = EDGE_LOOP ( 'NONE', ( #3714, #6625 ) ) ;
#3438 = CARTESIAN_POINT ( 'NONE',  ( 190.5000000000000568, -178.7362136002515172, -17.68580191161595394 ) ) ;
#3439 = ADVANCED_FACE ( 'NONE', ( #14540 ), #5236, .F. ) ;
#3440 = CARTESIAN_POINT ( 'NONE',  ( -199.4124801547868913, 127.6177204676982910, 1.515400478619089109 ) ) ;
#3443 = EDGE_CURVE ( 'NONE', #9203, #8894, #8565, .T. ) ;
#3442 = EDGE_CURVE ( 'NONE', #14585, #12671, #14624, .T. ) ;
#3441 = DIRECTION ( 'NONE',  ( -0.000000000000000000, 1.000000000000000000, 1.486905836551548832E-16 ) ) ;
#3444 = CARTESIAN_POINT ( 'NONE',  ( -152.4086188282879277, 107.2728346664360259, -5.000000000000000000 ) ) ;
#3445 = CIRCLE ( 'NONE', #5468, 3.525000000000002132 ) ;
#3446 = CARTESIAN_POINT ( 'NONE',  ( 205.4496313998743915, 47.84832575209421890, -7.060263518810960370 ) ) ;
#3447 = CIRCLE ( 'NONE', #653, 1.700000000000007061 ) ;
#3448 = EDGE_LOOP ( 'NONE', ( #10788, #8936, #4929, #9659 ) ) ;
#3449 = ORIENTED_EDGE ( 'NONE', *, *, #11312, .T. ) ;
#3450 = CARTESIAN_POINT ( 'NONE',  ( 202.3883256910358739, 32.65987148549056229, -8.116337980372584582 ) ) ;
#3451 = CARTESIAN_POINT ( 'NONE',  ( -86.77455057502459113, 65.19100426474074084, 0.000000000000000000 ) ) ;
#3452 = LINE ( 'NONE', #12836, #8924 ) ;
#3453 = CARTESIAN_POINT ( 'NONE',  ( -76.50000000000004263, -178.9449732516916072, 64.32815825124538378 ) ) ;
#3454 = CARTESIAN_POINT ( 'NONE',  ( -222.2186395530536629, 144.7337101510026116, -3.675081463328696341 ) ) ;
#3455 = CARTESIAN_POINT ( 'NONE',  ( -219.3831369218127065, 150.1479396093025684, 9.707727764924111824 ) ) ;
#3456 = CARTESIAN_POINT ( 'NONE',  ( -152.4086188282879277, 107.2728346664360259, 5.000000000000000000 ) ) ;
#3457 = CARTESIAN_POINT ( 'NONE',  ( -64.00000000000002842, 16.03993994372673981, 7.553451883674125344E-16 ) ) ;
#3458 = CARTESIAN_POINT ( 'NONE',  ( -35.99999999999995026, 64.53993994372673626, 15.00000000000139977 ) ) ;
#3459 = CARTESIAN_POINT ( 'NONE',  ( -3.916680348103880824E-15, -2.246824879981689005, 1.608385152161860621 ) ) ;
#3460 = DIRECTION ( 'NONE',  ( 0.000000000000000000, 0.000000000000000000, 1.000000000000000000 ) ) ;
#3461 = ORIENTED_EDGE ( 'NONE', *, *, #4189, .F. ) ;
#3462 = SHAPE_REPRESENTATION_RELATIONSHIP ( 'NONE' , 'NONE' ,  #13652, #10185 ) ;
#3463 = ORIENTED_EDGE ( 'NONE', *, *, #9811, .F. ) ;
#3464 = DIRECTION ( 'NONE',  ( 0.000000000000000000, 0.1391731009600660485, -0.9902680687415702510 ) ) ;
#3465 = CARTESIAN_POINT ( 'NONE',  ( -70.00000000000000000, -201.3058001507315566, -42.95141194869119516 ) ) ;
#3466 = DIRECTION ( 'NONE',  ( -1.000000000000000000, -0.000000000000000000, -0.000000000000000000 ) ) ;
#3467 = PLANE ( 'NONE',  #14027 ) ;
#3468 = ORIENTED_EDGE ( 'NONE', *, *, #13150, .F. ) ;
#3469 = EDGE_CURVE ( 'NONE', #1098, #8246, #10995, .T. ) ;
#3470 = CONTEXT_DEPENDENT_SHAPE_REPRESENTATION ( #7062, #14065 ) ;
#3471 = AXIS2_PLACEMENT_3D ( 'NONE', #10125, #14919, #12058 ) ;
#3472 = ORIENTED_EDGE ( 'NONE', *, *, #3139, .T. ) ;
#3473 = CARTESIAN_POINT ( 'NONE',  ( 201.4161383703745400, 32.18800505576257365, -3.749910732146560122 ) ) ;
#3474 = ORIENTED_EDGE ( 'NONE', *, *, #4716, .F. ) ;
#3475 = CARTESIAN_POINT ( 'NONE',  ( 14.00000000000004086, 64.53993994372673626, 18.52500000000105018 ) ) ;
#3476 = CARTESIAN_POINT ( 'NONE',  ( -223.5918188539070002, 142.0538562971642307, 1.612306317632525410 ) ) ;
#3477 = ORIENTED_EDGE ( 'NONE', *, *, #455, .F. ) ;
#3478 = VERTEX_POINT ( 'NONE', #3967 ) ;
#3479 = DIRECTION ( 'NONE',  ( -0.000000000000000000, 0.000000000000000000, 1.000000000000000000 ) ) ;
#3480 = DIRECTION ( 'NONE',  ( -0.000000000000000000, -4.956352788505162775E-17, 1.000000000000000000 ) ) ;
#3481 = ORIENTED_EDGE ( 'NONE', *, *, #10450, .F. ) ;
#3482 = VECTOR ( 'NONE', #12835, 1000.000000000000000 ) ;
#3483 = CARTESIAN_POINT ( 'NONE',  ( -150.8759110177108766, 106.3887477331416989, 9.406539233868651095 ) ) ;
#3484 = FACE_OUTER_BOUND ( 'NONE', #11779, .T. ) ;
#3485 = CIRCLE ( 'NONE', #2738, 1.219500000000000028 ) ;
#3486 = EDGE_CURVE ( 'NONE', #7029, #13870, #4163, .T. ) ;
#3487 = DIRECTION ( 'NONE',  ( -0.8660254037844388186, 0.4999999999999997780, 0.000000000000000000 ) ) ;
#3488 = VERTEX_POINT ( 'NONE', #7538 ) ;
#3489 = VECTOR ( 'NONE', #5079, 1000.000000000000000 ) ;
#3490 = LINE ( 'NONE', #15399, #12841 ) ;
#3491 = AXIS2_PLACEMENT_3D ( 'NONE', #12472, #1662, #3884 ) ;
#3492 = ORIENTED_EDGE ( 'NONE', *, *, #2047, .F. ) ;
#3493 = ADVANCED_FACE ( 'NONE', ( #12334 ), #1285, .T. ) ;
#3494 = CARTESIAN_POINT ( 'NONE',  ( -88.77455057502459113, 65.19100426474074084, 7.600000000000002309 ) ) ;
#3495 = AXIS2_PLACEMENT_3D ( 'NONE', #1918, #13843, #6446 ) ;
#3496 = DIRECTION ( 'NONE',  ( -0.000000000000000000, -0.000000000000000000, 1.000000000000000000 ) ) ;
#3497 = CARTESIAN_POINT ( 'NONE',  ( 170.8293059057019718, 61.25683321636181233, 10.00000000000000178 ) ) ;
#3498 = ORIENTED_EDGE ( 'NONE', *, *, #9348, .T. ) ;
#3499 = CARTESIAN_POINT ( 'NONE',  ( -218.4400809351218413, 155.8695184890967482, 1.515441477806783510 ) ) ;
#3500 = ADVANCED_FACE ( 'NONE', ( #91 ), #3419, .T. ) ;
#3501 = CARTESIAN_POINT ( 'NONE',  ( 201.8412736707888087, 29.11599755995149152, -3.759251452247287517 ) ) ;
#3502 = ORIENTED_EDGE ( 'NONE', *, *, #2661, .T. ) ;
#3503 = FACE_BOUND ( 'NONE', #13506, .T. ) ;
#3504 = CARTESIAN_POINT ( 'NONE',  ( 184.0000000000000568, -181.3058001507315566, -41.45141194869120227 ) ) ;
#3505 = AXIS2_PLACEMENT_3D ( 'NONE', #10343, #13968, #11607 ) ;
#3506 = DIRECTION ( 'NONE',  ( 0.000000000000000000, 0.000000000000000000, -1.000000000000000000 ) ) ;
#3507 = AXIS2_PLACEMENT_3D ( 'NONE', #884, #9202, #9276 ) ;
#3508 = ADVANCED_FACE ( 'NONE', ( #1361 ), #10060, .F. ) ;
#3509 = VERTEX_POINT ( 'NONE', #13592 ) ;
#3510 = CARTESIAN_POINT ( 'NONE',  ( 184.0000000000000568, 21.53993994372674337, -12.49999999999999645 ) ) ;
#3511 = DIRECTION ( 'NONE',  ( 0.000000000000000000, 0.000000000000000000, 1.000000000000000000 ) ) ;
#3512 = CARTESIAN_POINT ( 'NONE',  ( 202.3883256910358739, 32.65987148549056229, -8.116337980372584582 ) ) ;
#3513 = ORIENTED_EDGE ( 'NONE', *, *, #4556, .F. ) ;
#3514 = DIRECTION ( 'NONE',  ( 1.077120774387149835E-15, -0.9902680687415711391, 0.1391731009600592484 ) ) ;
#3515 = LINE ( 'NONE', #2250, #8965 ) ;
#3516 = CARTESIAN_POINT ( 'NONE',  ( -181.9060177919747048, 118.7341819232202909, 5.367833425961690885 ) ) ;
#3517 = CARTESIAN_POINT ( 'NONE',  ( -156.6477983077465410, 110.1970436846185066, 84.88378295107887084 ) ) ;
#3518 = CARTESIAN_POINT ( 'NONE',  ( 203.7481738146713326, 51.76374178194004827, -0.9107274384406881529 ) ) ;
#3519 = FACE_OUTER_BOUND ( 'NONE', #9583, .T. ) ;
#3520 = ORIENTED_EDGE ( 'NONE', *, *, #3443, .T. ) ;
#3521 = APPLICATION_CONTEXT ( 'automotive_design' ) ;
#3522 = EDGE_LOOP ( 'NONE', ( #15265, #15251 ) ) ;
#3523 = CARTESIAN_POINT ( 'NONE',  ( -76.50000000000001421, -179.8058001507315566, -17.19066787724516843 ) ) ;
#3524 = FACE_BOUND ( 'NONE', #2902, .T. ) ;
#3525 = ADVANCED_FACE ( 'NONE', ( #2800 ), #6198, .F. ) ;
#3526 = DIRECTION ( 'NONE',  ( -1.000000000000000000, 0.000000000000000000, 0.000000000000000000 ) ) ;
#3527 = DIRECTION ( 'NONE',  ( 0.000000000000000000, 0.000000000000000000, -1.000000000000000000 ) ) ;
#3528 = CIRCLE ( 'NONE', #2778, 0.4999999999999998890 ) ;
#3529 = CARTESIAN_POINT ( 'NONE',  ( -223.4760924884873248, 146.8467132707474434, -4.490349463211885883 ) ) ;
#3530 = AXIS2_PLACEMENT_3D ( 'NONE', #13518, #8724, #9993 ) ;
#3531 = VECTOR ( 'NONE', #1563, 1000.000000000000000 ) ;
#3532 = EDGE_CURVE ( 'NONE', #6607, #8299, #1601, .T. ) ;
#3533 = EDGE_CURVE ( 'NONE', #8499, #9526, #13673, .T. ) ;
#3534 = CARTESIAN_POINT ( 'NONE',  ( -217.8113179378289317, 152.9593294075854431, 7.845513341075405656 ) ) ;
#3535 = AXIS2_PLACEMENT_3D ( 'NONE', #12958, #1986, #9195 ) ;
#3536 = DIRECTION ( 'NONE',  ( 1.000000000000000000, 0.000000000000000000, 0.000000000000000000 ) ) ;
#3537 = EDGE_CURVE ( 'NONE', #5369, #15306, #8961, .T. ) ;
#3538 = DIRECTION ( 'NONE',  ( 0.000000000000000000, 0.000000000000000000, -1.000000000000000000 ) ) ;
#3539 = DIRECTION ( 'NONE',  ( 0.000000000000000000, 2.775557561562888827E-14, 1.000000000000000000 ) ) ;
#3540 = PLANE ( 'NONE',  #13909 ) ;
#3541 = ORIENTED_EDGE ( 'NONE', *, *, #11754, .F. ) ;
#3542 = ORIENTED_EDGE ( 'NONE', *, *, #5274, .T. ) ;
#3543 = DIRECTION ( 'NONE',  ( 1.000000000000000000, 0.000000000000000000, 0.000000000000000000 ) ) ;
#3544 = CARTESIAN_POINT ( 'NONE',  ( 190.0000000000000853, 15.17911304468679745, 25.93769382960994818 ) ) ;
#3545 = DIRECTION ( 'NONE',  ( 0.000000000000000000, 0.000000000000000000, 1.000000000000000000 ) ) ;
#3546 = FACE_BOUND ( 'NONE', #4034, .T. ) ;
#3547 = DIRECTION ( 'NONE',  ( -1.000000000000000000, 0.000000000000000000, 0.000000000000000000 ) ) ;
#3548 = LINE ( 'NONE', #3256, #9749 ) ;
#3549 = ADVANCED_FACE ( 'NONE', ( #14931 ), #2955, .F. ) ;
#3550 = ADVANCED_FACE ( 'NONE', ( #10290, #5631 ), #7700, .F. ) ;
#3551 = AXIS2_PLACEMENT_3D ( 'NONE', #6958, #854, #8069 ) ;
#3552 = VERTEX_POINT ( 'NONE', #6515 ) ;
#3553 = VECTOR ( 'NONE', #3927, 1000.000000000000000 ) ;
#3554 = VERTEX_POINT ( 'NONE', #6676 ) ;
#3555 = CARTESIAN_POINT ( 'NONE',  ( 205.4496313998743915, 47.84832575209421890, -7.060263518810960370 ) ) ;
#3556 = FACE_OUTER_BOUND ( 'NONE', #14843, .T. ) ;
#3557 = ORIENTED_EDGE ( 'NONE', *, *, #1390, .F. ) ;
#3558 = DIRECTION ( 'NONE',  ( 0.000000000000000000, 0.000000000000000000, 1.000000000000000000 ) ) ;
#3559 = CARTESIAN_POINT ( 'NONE',  ( -223.3756880201893580, 142.5055725410610705, 5.363114072299179469 ) ) ;
#3560 = ORIENTED_EDGE ( 'NONE', *, *, #6190, .F. ) ;
#3561 = VERTEX_POINT ( 'NONE', #640 ) ;
#3562 = CARTESIAN_POINT ( 'NONE',  ( 5.799999999999999822, 9.237604307034018802, 0.000000000000000000 ) ) ;
#3563 = CARTESIAN_POINT ( 'NONE',  ( 5.799999999999999822, 4.618802153516981868, 8.000000000000007105 ) ) ;
#3564 = CIRCLE ( 'NONE', #9622, 2.000000000000002220 ) ;
#3565 = ADVANCED_FACE ( 'NONE', ( #7774 ), #3179, .F. ) ;
#3566 = ORIENTED_EDGE ( 'NONE', *, *, #13771, .F. ) ;
#3567 = DIRECTION ( 'NONE',  ( -0.4873681696970817989, -0.8731965799097684000, 0.000000000000000000 ) ) ;
#3568 = CARTESIAN_POINT ( 'NONE',  ( 190.0000000000000568, 16.03993994372673981, 10.05257423913146475 ) ) ;
#3569 = COLOUR_RGB ( '', 0.40784314, 0.44705882, 0.49803922) ;
#3570 = DIRECTION ( 'NONE',  ( 0.000000000000000000, 0.000000000000000000, 1.000000000000000000 ) ) ;
#3571 = VERTEX_POINT ( 'NONE', #15009 ) ;
#3572 = ORIENTED_EDGE ( 'NONE', *, *, #7804, .F. ) ;
#3573 = VECTOR ( 'NONE', #12281, 1000.000000000000000 ) ;
#3574 = ORIENTED_EDGE ( 'NONE', *, *, #7254, .F. ) ;
#3575 = DIRECTION ( 'NONE',  ( 0.000000000000000000, 0.000000000000000000, 1.000000000000000000 ) ) ;
#3576 = CARTESIAN_POINT ( 'NONE',  ( 13.07968152355895874, 460.3807876674321165, 5.000000000000000000 ) ) ;
#3577 = EDGE_CURVE ( 'NONE', #6971, #7619, #13751, .T. ) ;
#3578 = DIRECTION ( 'NONE',  ( 0.000000000000000000, 0.000000000000000000, 1.000000000000000000 ) ) ;
#3579 = ORIENTED_EDGE ( 'NONE', *, *, #3920, .T. ) ;
#3580 = ORIENTED_EDGE ( 'NONE', *, *, #13086, .F. ) ;
#3581 = CARTESIAN_POINT ( 'NONE',  ( -206.2168697392640695, 148.5706983463157940, -0.4547266291960757045 ) ) ;
#3582 = UNCERTAINTY_MEASURE_WITH_UNIT (LENGTH_MEASURE( 1.000000000000000082E-05 ), #13313, 'distance_accuracy_value', 'NONE');
#3583 = CARTESIAN_POINT ( 'NONE',  ( 209.5402858782260864, 48.07700032709870896, -2.761241636875660710 ) ) ;
#3584 = ADVANCED_BREP_SHAPE_REPRESENTATION ( '', ( #269, #12337 ), #11555 ) ;
#3585 = ORIENTED_EDGE ( 'NONE', *, *, #2661, .F. ) ;
#3586 = EDGE_CURVE ( 'NONE', #11697, #12019, #9247, .T. ) ;
#3587 = DIRECTION ( 'NONE',  ( 0.000000000000000000, 0.1391731009600584990, -0.9902680687415712502 ) ) ;
#3588 = LINE ( 'NONE', #8421, #7225 ) ;
#3589 = DIRECTION ( 'NONE',  ( -1.000000000000000000, 0.000000000000000000, 0.000000000000000000 ) ) ;
#3590 = ORIENTED_EDGE ( 'NONE', *, *, #1602, .T. ) ;
#3591 = SHAPE_DEFINITION_REPRESENTATION ( #11691, #12546 ) ;
#3592 = CARTESIAN_POINT ( 'NONE',  ( 177.5000000000000853, 17.53993994372673981, -17.50000000000002487 ) ) ;
#3593 = CARTESIAN_POINT ( 'NONE',  ( 201.8629198063431716, 32.54887535240757757, -8.146526315903498627 ) ) ;
#3594 = EDGE_LOOP ( 'NONE', ( #1330, #13326, #7221, #14882 ) ) ;
#3595 = FACE_OUTER_BOUND ( 'NONE', #4043, .T. ) ;
#3596 = DIRECTION ( 'NONE',  ( 0.000000000000000000, 0.9902680687415702510, 0.1391731009600660485 ) ) ;
#3597 = CARTESIAN_POINT ( 'NONE',  ( -191.4964613557999655, 125.7493975051623352, 1.515400478619084224 ) ) ;
#3598 = DIRECTION ( 'NONE',  ( 0.000000000000000000, 0.000000000000000000, -1.000000000000000000 ) ) ;
#3599 = EDGE_LOOP ( 'NONE', ( #3360, #9569, #3619 ) ) ;
#3600 = CARTESIAN_POINT ( 'NONE',  ( -209.3130641152695830, 145.0632059852189570, 9.578254705571840333 ) ) ;
#3601 = AXIS2_PLACEMENT_3D ( 'NONE', #1345, #14448, #15543 ) ;
#3602 = FACE_OUTER_BOUND ( 'NONE', #11632, .T. ) ;
#3603 = ORIENTED_EDGE ( 'NONE', *, *, #7385, .T. ) ;
#3604 = VERTEX_POINT ( 'NONE', #13832 ) ;
#3605 = DIRECTION ( 'NONE',  ( -0.000000000000000000, -0.000000000000000000, -1.000000000000000000 ) ) ;
#3606 = LINE ( 'NONE', #10637, #11600 ) ;
#3607 = LINE ( 'NONE', #1306, #9183 ) ;
#3608 = LINE ( 'NONE', #4631, #9248 ) ;
#3609 = LINE ( 'NONE', #5980, #15367 ) ;
#3610 = CARTESIAN_POINT ( 'NONE',  ( -151.4086188282879277, 107.2728346664360259, -5.000000000000000000 ) ) ;
#3611 = VECTOR ( 'NONE', #3378, 1000.000000000000000 ) ;
#3612 = CYLINDRICAL_SURFACE ( 'NONE', #1091, 5.000000000000004441 ) ;
#3613 = CARTESIAN_POINT ( 'NONE',  ( -157.6477983077465694, 110.1970436846184924, 9.411501811869198875 ) ) ;
#3614 = CIRCLE ( 'NONE', #7185, 1.700000000000001954 ) ;
#3615 = FACE_OUTER_BOUND ( 'NONE', #10833, .T. ) ;
#3616 = DIRECTION ( 'NONE',  ( 0.000000000000000000, 0.000000000000000000, -1.000000000000000000 ) ) ;
#3617 = EDGE_LOOP ( 'NONE', ( #5705, #3268 ) ) ;
#3618 = ADVANCED_FACE ( 'NONE', ( #476 ), #1680, .F. ) ;
#3619 = ORIENTED_EDGE ( 'NONE', *, *, #14144, .T. ) ;
#3620 = DIRECTION ( 'NONE',  ( -1.000000000000000000, -0.000000000000000000, -0.000000000000000000 ) ) ;
#3621 = FACE_OUTER_BOUND ( 'NONE', #13646, .T. ) ;
#3622 = VECTOR ( 'NONE', #11031, 1000.000000000000000 ) ;
#3623 = DIRECTION ( 'NONE',  ( -1.000000000000000000, 0.000000000000000000, 0.000000000000000000 ) ) ;
#3624 = LINE ( 'NONE', #2677, #8665 ) ;
#3625 = LINE ( 'NONE', #13241, #13776 ) ;
#3626 = CARTESIAN_POINT ( 'NONE',  ( -35.99999999999995026, 64.53993994372673626, 18.52500000000140190 ) ) ;
#3627 = CARTESIAN_POINT ( 'NONE',  ( -193.7200834347810599, 142.0619459586758921, 2.500000000000000000 ) ) ;
#3628 = ORIENTED_EDGE ( 'NONE', *, *, #3413, .T. ) ;
#3629 = ORIENTED_EDGE ( 'NONE', *, *, #3442, .T. ) ;
#3630 = CIRCLE ( 'NONE', #14201, 1.700000000000007061 ) ;
#3631 = ORIENTED_EDGE ( 'NONE', *, *, #9662, .F. ) ;
#3632 = ADVANCED_FACE ( 'NONE', ( #12647 ), #13917, .F. ) ;
#3633 = ADVANCED_FACE ( 'NONE', ( #3032 ), #7937, .T. ) ;
#3634 = AXIS2_PLACEMENT_3D ( 'NONE', #14195, #11917, #9474 ) ;
#3635 = EDGE_CURVE ( 'NONE', #8082, #3571, #11315, .T. ) ;
#3636 = CARTESIAN_POINT ( 'NONE',  ( -223.1853449316457159, 142.8873074582503193, 6.221962389395381265 ) ) ;
#3637 = ORIENTED_EDGE ( 'NONE', *, *, #6614, .T. ) ;
#3638 = EDGE_LOOP ( 'NONE', ( #11666, #12162, #10756, #4770 ) ) ;
#3639 = LINE ( 'NONE', #7796, #3988 ) ;
#3640 = LINE ( 'NONE', #2381, #9118 ) ;
#3641 = ORIENTED_EDGE ( 'NONE', *, *, #11588, .T. ) ;
#3642 = CARTESIAN_POINT ( 'NONE',  ( 201.7746181419471725, 32.40197136543856971, -7.616432591815856412 ) ) ;
#3643 = CARTESIAN_POINT ( 'NONE',  ( -63.50000000000002842, -179.3058001507315566, 65.31842631998698323 ) ) ;
#3644 = LINE ( 'NONE', #10843, #2589 ) ;
#3645 = ADVANCED_FACE ( 'NONE', ( #4195 ), #11508, .F. ) ;
#3646 = ORIENTED_EDGE ( 'NONE', *, *, #3187, .F. ) ;
#3647 = DIRECTION ( 'NONE',  ( 0.4147405137080060755, -0.9099397267342597129, 0.000000000000000000 ) ) ;
#3648 = VERTEX_POINT ( 'NONE', #4357 ) ;
#3649 = LINE ( 'NONE', #959, #1133 ) ;
#3650 = CIRCLE ( 'NONE', #8213, 1.000000000000000888 ) ;
#3651 = CARTESIAN_POINT ( 'NONE',  ( -218.4444600228138711, 155.8616726660956715, 2.500000000270498735 ) ) ;
#3652 = CARTESIAN_POINT ( 'NONE',  ( -150.4342454288345721, 107.5345008671435920, -4.906289360893212326 ) ) ;
#3653 = ORIENTED_EDGE ( 'NONE', *, *, #10887, .F. ) ;
#3654 = EDGE_LOOP ( 'NONE', ( #4120, #5910, #4456, #3080 ) ) ;
#3655 = CARTESIAN_POINT ( 'NONE',  ( -206.0135413368010404, 148.9337379340180405, 1.515441477536285220 ) ) ;
#3656 = CARTESIAN_POINT ( 'NONE',  ( 205.3436520073863107, 47.91354567463725544, -5.626644267508417840 ) ) ;
#3657 = EDGE_LOOP ( 'NONE', ( #12916, #10360, #4408, #5195, #10618, #11788 ) ) ;
#3658 = DIRECTION ( 'NONE',  ( -1.000000000000000000, 0.000000000000000000, 0.000000000000000000 ) ) ;
#3659 = FACE_BOUND ( 'NONE', #368, .T. ) ;
#3660 = CARTESIAN_POINT ( 'NONE',  ( 64.00000000000005684, 64.53993994372673626, 11.47500000000070131 ) ) ;
#3661 = AXIS2_PLACEMENT_3D ( 'NONE', #2390, #11950, #3420 ) ;
#3662 = EDGE_CURVE ( 'NONE', #435, #13457, #8012, .T. ) ;
#3663 = EDGE_LOOP ( 'NONE', ( #11878, #8174 ) ) ;
#3664 = EDGE_CURVE ( 'NONE', #10667, #3488, #12798, .T. ) ;
#3665 = CARTESIAN_POINT ( 'NONE',  ( 0.08224679563969686247, 6.145890662064630305, -5.355005115540884653 ) ) ;
#3666 = CARTESIAN_POINT ( 'NONE',  ( 205.4107168461011099, 33.83372868983673243, -6.361989640121679557 ) ) ;
#3667 = ORIENTED_EDGE ( 'NONE', *, *, #10642, .T. ) ;
#3668 = CARTESIAN_POINT ( 'NONE',  ( 0.000000000000000000, 0.000000000000000000, 0.000000000000000000 ) ) ;
#3669 = DIRECTION ( 'NONE',  ( -0.000000000000000000, -0.000000000000000000, -1.000000000000000000 ) ) ;
#3670 = CARTESIAN_POINT ( 'NONE',  ( -205.7735142771631160, 131.5899501701119334, 5.434137442415934771 ) ) ;
#3671 = CARTESIAN_POINT ( 'NONE',  ( 178.0000000000000853, 21.51947656765318229, 9.953386152224130257 ) ) ;
#3672 = EDGE_LOOP ( 'NONE', ( #6926, #303, #10523, #3929 ) ) ;
#3673 = CARTESIAN_POINT ( 'NONE',  ( -179.6920193139674780, 128.7453118898713456, 9.578254705571842109 ) ) ;
#3674 = FACE_OUTER_BOUND ( 'NONE', #2771, .T. ) ;
#3675 = AXIS2_PLACEMENT_3D ( 'NONE', #11931, #9485, #11855 ) ;
#3676 = ORIENTED_EDGE ( 'NONE', *, *, #7183, .F. ) ;
#3677 = ORIENTED_EDGE ( 'NONE', *, *, #11806, .F. ) ;
#3678 = DIRECTION ( 'NONE',  ( 0.000000000000000000, 0.000000000000000000, -1.000000000000000000 ) ) ;
#3679 = AXIS2_PLACEMENT_3D ( 'NONE', #6438, #398, #6357 ) ;
#3680 = CARTESIAN_POINT ( 'NONE',  ( 200.1062858801516597, 47.86394065090266992, 10.00000000000000533 ) ) ;
#3681 = DIRECTION ( 'NONE',  ( -0.000000000000000000, -0.9902680687415712502, -0.1391731009600586100 ) ) ;
#3682 = CARTESIAN_POINT ( 'NONE',  ( 122.5806775638430253, 45.00321902537314145, 10.00000000000000178 ) ) ;
#3683 = CARTESIAN_POINT ( 'NONE',  ( -150.4086188282879277, 107.2728346664360259, 0.000000000000000000 ) ) ;
#3684 = CARTESIAN_POINT ( 'NONE',  ( -110.0000000000000426, 19.53993994372674337, 24.99999999999999645 ) ) ;
#3685 = AXIS2_PLACEMENT_3D ( 'NONE', #10140, #6086, #128 ) ;
#3686 = DIRECTION ( 'NONE',  ( -0.000000000000000000, 0.9902680687415713612, -0.1391731009600582492 ) ) ;
#3687 = CIRCLE ( 'NONE', #11259, 0.5000000000000004441 ) ;
#3688 = CARTESIAN_POINT ( 'NONE',  ( 14.00000000000004086, 62.13993994372673768, 11.50000000000105160 ) ) ;
#3689 = CARTESIAN_POINT ( 'NONE',  ( 177.5000000000000853, -179.3753867012115961, -29.38864891670827362 ) ) ;
#3690 = ORIENTED_EDGE ( 'NONE', *, *, #8722, .T. ) ;
#3691 = ADVANCED_FACE ( 'NONE', ( #9268 ), #1667, .T. ) ;
#3692 = DIRECTION ( 'NONE',  ( 0.000000000000000000, 0.000000000000000000, 1.000000000000000000 ) ) ;
#3693 = SHAPE_REPRESENTATION_RELATIONSHIP ( 'NONE' , 'NONE' ,  #10258, #2066 ) ;
#3694 = ORIENTED_EDGE ( 'NONE', *, *, #14509, .F. ) ;
#3695 = DIRECTION ( 'NONE',  ( -1.000000000000000000, 0.000000000000000000, 0.000000000000000000 ) ) ;
#3696 = CARTESIAN_POINT ( 'NONE',  ( -70.00000000000000000, 15.53993994372673626, 47.49999999999997868 ) ) ;
#3697 = CARTESIAN_POINT ( 'NONE',  ( -171.4541674549778918, 121.0456171749203662, 2.431557144026069928 ) ) ;
#3698 =( LENGTH_UNIT ( ) NAMED_UNIT ( * ) SI_UNIT ( .MILLI., .METRE. ) );
#3699 = LINE ( 'NONE', #13084, #5721 ) ;
#3700 = EDGE_CURVE ( 'NONE', #319, #6121, #5316, .T. ) ;
#3701 = AXIS2_PLACEMENT_3D ( 'NONE', #5840, #13402, #2600 ) ;
#3702 = DIRECTION ( 'NONE',  ( -0.000000000000000000, 1.000000000000000000, -0.000000000000000000 ) ) ;
#3703 = CARTESIAN_POINT ( 'NONE',  ( -201.8658614229783268, 146.6084512934502584, 2.500000000000000000 ) ) ;
#3704 = VERTEX_POINT ( 'NONE', #12223 ) ;
#3705 = EDGE_CURVE ( 'NONE', #12666, #13605, #5710, .T. ) ;
#3706 = ORIENTED_EDGE ( 'NONE', *, *, #4142, .T. ) ;
#3707 = CARTESIAN_POINT ( 'NONE',  ( 194.7786688470199010, 47.83282381504752578, -5.005399988216014506 ) ) ;
#3708 = DIRECTION ( 'NONE',  ( -1.000000000000000000, 0.000000000000000000, 0.000000000000000000 ) ) ;
#3709 = VERTEX_POINT ( 'NONE', #13405 ) ;
#3710 = CARTESIAN_POINT ( 'NONE',  ( -222.6541231320287579, 148.3194004002985196, 7.781232655114622254 ) ) ;
#3711 = ORIENTED_EDGE ( 'NONE', *, *, #14847, .F. ) ;
#3712 = CARTESIAN_POINT ( 'NONE',  ( -162.5597267027908401, 124.6703825060609745, 2.431557144026069928 ) ) ;
#3713 = CARTESIAN_POINT ( 'NONE',  ( 207.3230658017955932, 31.40903172769477081, -1.939356299889454016 ) ) ;
#3714 = ORIENTED_EDGE ( 'NONE', *, *, #8427, .F. ) ;
#3715 = DIRECTION ( 'NONE',  ( 1.000000000000000000, 0.000000000000000000, 0.000000000000000000 ) ) ;
#3716 = DIRECTION ( 'NONE',  ( 0.000000000000000000, 0.000000000000000000, -1.000000000000000000 ) ) ;
#3717 = EDGE_CURVE ( 'NONE', #15409, #14286, #7742, .T. ) ;
#3718 = DIRECTION ( 'NONE',  ( -0.3662838836490099337, 0.9305003370641709015, 0.002288952263120960697 ) ) ;
#3719 = ORIENTED_EDGE ( 'NONE', *, *, #14625, .F. ) ;
#3720 = CIRCLE ( 'NONE', #3973, 0.5000000000000004441 ) ;
#3722 = EDGE_CURVE ( 'NONE', #14758, #8929, #4955, .T. ) ;
#3721 = EDGE_CURVE ( 'NONE', #7132, #8246, #3548, .T. ) ;
#3723 = ORIENTED_EDGE ( 'NONE', *, *, #9522, .F. ) ;
#3724 =( NAMED_UNIT ( * ) PLANE_ANGLE_UNIT ( ) SI_UNIT ( $, .RADIAN. ) );
#3725 = ADVANCED_FACE ( 'NONE', ( #8096 ), #12071, .F. ) ;
#3726 = CARTESIAN_POINT ( 'NONE',  ( 177.5000000000000853, 15.17911304468679745, 25.93769382960995884 ) ) ;
#3727 = EDGE_LOOP ( 'NONE', ( #15081, #12045 ) ) ;
#3728 = DIRECTION ( 'NONE',  ( 0.000000000000000000, 0.000000000000000000, -1.000000000000000000 ) ) ;
#3729 = CIRCLE ( 'NONE', #14557, 5.000000000000017764 ) ;
#3730 = CARTESIAN_POINT ( 'NONE',  ( -150.4086188282878425, 107.4035458162468331, -4.884442077755429601 ) ) ;
#3731 = VERTEX_POINT ( 'NONE', #13244 ) ;
#3732 = EDGE_LOOP ( 'NONE', ( #12108, #1204 ) ) ;
#3733 = CARTESIAN_POINT ( 'NONE',  ( -207.9521514620915639, 147.4834172152791325, -2.963320117457100888 ) ) ;
#3734 = DIRECTION ( 'NONE',  ( -0.000000000000000000, -0.000000000000000000, -1.000000000000000000 ) ) ;
#3735 = CIRCLE ( 'NONE', #7030, 0.4999999999999996114 ) ;
#3736 = EDGE_LOOP ( 'NONE', ( #11688, #13847, #11326, #13585 ) ) ;
#3737 = DIRECTION ( 'NONE',  ( -1.000000000000000000, 0.000000000000000000, 0.000000000000000000 ) ) ;
#3738 = DIRECTION ( 'NONE',  ( -5.518327896226369609E-17, -0.9902680687415712502, -0.1391731009600584990 ) ) ;
#3739 = DIRECTION ( 'NONE',  ( 0.5602235199536453880, 0.8138631617988981715, 0.1541958545404129299 ) ) ;
#3740 = EDGE_CURVE ( 'NONE', #14616, #2142, #13555, .T. ) ;
#3741 = AXIS2_PLACEMENT_3D ( 'NONE', #4266, #11780, #946 ) ;
#3742 = EDGE_LOOP ( 'NONE', ( #9867, #8103, #13264, #5637, #1035 ) ) ;
#3743 = DIRECTION ( 'NONE',  ( 1.000000000000000000, 0.000000000000000000, 0.000000000000000000 ) ) ;
#3744 = VECTOR ( 'NONE', #4132, 1000.000000000000000 ) ;
#3745 = DIRECTION ( 'NONE',  ( -0.000000000000000000, 1.000000000000000000, -0.000000000000000000 ) ) ;
#3746 = CARTESIAN_POINT ( 'NONE',  ( 193.0268458394156710, 50.40397125358524733, -1.873914241081319210 ) ) ;
#3747 = ORIENTED_EDGE ( 'NONE', *, *, #7881, .T. ) ;
#3748 = LINE ( 'NONE', #3833, #12138 ) ;
#3749 = CARTESIAN_POINT ( 'NONE',  ( 66.74035645333923128, 38.79159067395544014, 10.00000000000000178 ) ) ;
#3750 = EDGE_CURVE ( 'NONE', #9812, #15306, #9801, .T. ) ;
#3751 = CARTESIAN_POINT ( 'NONE',  ( -190.6388552492889517, 127.3288340616119143, -2.964974570226841522 ) ) ;
#3752 = CARTESIAN_POINT ( 'NONE',  ( -85.27455057502459113, 65.19100426474074084, 5.000000000000000000 ) ) ;
#3753 = ORIENTED_EDGE ( 'NONE', *, *, #4567, .F. ) ;
#3754 = CARTESIAN_POINT ( 'NONE',  ( -211.5791133502170283, 138.9897555992265268, 9.577123744044227394 ) ) ;
#3755 = CARTESIAN_POINT ( 'NONE',  ( 2.000000000000000000, -1.587713240271472648, -2.750000000000000888 ) ) ;
#3756 = VERTEX_POINT ( 'NONE', #14432 ) ;
#3757 = ORIENTED_EDGE ( 'NONE', *, *, #6516, .F. ) ;
#3758 = CIRCLE ( 'NONE', #9790, 1.700000000000000178 ) ;
#3759 = CARTESIAN_POINT ( 'NONE',  ( 0.000000000000000000, 0.000000000000000000, 0.000000000000000000 ) ) ;
#3760 = LINE ( 'NONE', #4193, #7841 ) ;
#3761 = AXIS2_PLACEMENT_3D ( 'NONE', #11469, #13584, #14767 ) ;
#3762 = EDGE_CURVE ( 'NONE', #6134, #10091, #8608, .T. ) ;
#3763 = DIRECTION ( 'NONE',  ( 0.000000000000000000, 0.000000000000000000, -1.000000000000000000 ) ) ;
#3764 = DIRECTION ( 'NONE',  ( 1.000000000000000000, -0.000000000000000000, -0.000000000000000000 ) ) ;
#3765 = CARTESIAN_POINT ( 'NONE',  ( -224.4522725255073397, 145.0977335000406470, 0.6248101478677640097 ) ) ;
#3766 = VECTOR ( 'NONE', #7075, 1000.000000000000000 ) ;
#3767 = DIRECTION ( 'NONE',  ( 0.000000000000000000, 0.000000000000000000, -1.000000000000000000 ) ) ;
#3768 = DIRECTION ( 'NONE',  ( 1.000000000000000000, 0.000000000000000000, 0.000000000000000000 ) ) ;
#3769 = CIRCLE ( 'NONE', #14339, 5.000000000000004441 ) ;
#3770 = DIRECTION ( 'NONE',  ( 0.000000000000000000, 0.000000000000000000, 1.000000000000000000 ) ) ;
#3771 = DIRECTION ( 'NONE',  ( -0.000000000000000000, 1.000000000000000000, 6.938893903907227145E-17 ) ) ;
#3772 = ORIENTED_EDGE ( 'NONE', *, *, #3221, .F. ) ;
#3773 = ORIENTED_EDGE ( 'NONE', *, *, #6054, .T. ) ;
#3774 = AXIS2_PLACEMENT_3D ( 'NONE', #423, #1858, #1705 ) ;
#3775 = DIRECTION ( 'NONE',  ( 0.000000000000000000, 0.7071067811865474617, 0.7071067811865474617 ) ) ;
#3776 = CARTESIAN_POINT ( 'NONE',  ( 177.5000000000000853, 15.53993994372673981, -17.50000000000002487 ) ) ;
#3777 = VECTOR ( 'NONE', #12339, 1000.000000000000000 ) ;
#3778 = DIRECTION ( 'NONE',  ( -0.000000000000000000, -0.000000000000000000, 1.000000000000000000 ) ) ;
#3779 = CIRCLE ( 'NONE', #6051, 2.000000000000001776 ) ;
#3780 = DIRECTION ( 'NONE',  ( 0.000000000000000000, -1.000000000000000000, -4.956352788505160310E-17 ) ) ;
#3781 = FACE_BOUND ( 'NONE', #6342, .T. ) ;
#3782 = ADVANCED_FACE ( 'NONE', ( #58 ), #2979, .T. ) ;
#3783 = CIRCLE ( 'NONE', #5797, 1.500000000000001332 ) ;
#3784 = CARTESIAN_POINT ( 'NONE',  ( -64.00000000000002842, -178.8058001507315566, 65.31842631998698323 ) ) ;
#3785 = CARTESIAN_POINT ( 'NONE',  ( 5.799999999999999822, 0.000000000000000000, 0.000000000000000000 ) ) ;
#3786 = ORIENTED_EDGE ( 'NONE', *, *, #2262, .T. ) ;
#3787 = AXIS2_PLACEMENT_3D ( 'NONE', #8092, #4432, #13990 ) ;
#3788 = AXIS2_PLACEMENT_3D ( 'NONE', #6789, #4405, #11441 ) ;
#3789 = ORIENTED_EDGE ( 'NONE', *, *, #13568, .T. ) ;
#3790 = AXIS2_PLACEMENT_3D ( 'NONE', #1623, #10008, #8740 ) ;
#3791 = CARTESIAN_POINT ( 'NONE',  ( 208.8010691282704840, 42.12517885095529380, -3.002821972062079681 ) ) ;
#3792 = CARTESIAN_POINT ( 'NONE',  ( -219.9686238450918552, 153.1308939251236154, 5.827571112376363160 ) ) ;
#3793 = VERTEX_POINT ( 'NONE', #10052 ) ;
#3794 = CARTESIAN_POINT ( 'NONE',  ( -220.5676733911498388, 147.9555285791823849, 9.924366136672199801 ) ) ;
#3795 = ORIENTED_EDGE ( 'NONE', *, *, #12897, .T. ) ;
#3796 = CARTESIAN_POINT ( 'NONE',  ( 178.0000000000000853, 15.53993994372673981, 9.617930870223348805 ) ) ;
#3797 = CARTESIAN_POINT ( 'NONE',  ( 201.7287634318787752, 52.64281578357326907, -6.816045903392632610 ) ) ;
#3798 = EDGE_CURVE ( 'NONE', #10971, #2355, #13054, .T. ) ;
#3799 = EDGE_LOOP ( 'NONE', ( #7251, #8804, #7770, #8689 ) ) ;
#3800 = CARTESIAN_POINT ( 'NONE',  ( 178.0000000000000853, -178.8058001507315566, -30.31842631998718574 ) ) ;
#3801 = DIRECTION ( 'NONE',  ( -0.000000000000000000, -0.000000000000000000, 1.000000000000000000 ) ) ;
#3802 = VECTOR ( 'NONE', #15060, 1000.000000000000000 ) ;
#3803 = B_SPLINE_CURVE_WITH_KNOTS ( 'NONE', 3,
 ( #12854, #9394, #7034, #14194, #1012, #3393 ),
 .UNSPECIFIED., .F., .F.,
 ( 4, 2, 4 ),
 ( 2.380731629935478318E-07, 0.002336973833157605842, 0.004673709593152217297 ),
 .UNSPECIFIED. ) ;
#3804 = ADVANCED_FACE ( 'NONE', ( #3023 ), #10211, .F. ) ;
#3805 = CIRCLE ( 'NONE', #13115, 1.499999999999996891 ) ;
#3806 = SHAPE_REPRESENTATION ( 'Lower Fixed Bed Shear Blade', ( #12337 ), #4262 ) ;
#3807 = LINE ( 'NONE', #7294, #10160 ) ;
#3808 = ORIENTED_EDGE ( 'NONE', *, *, #5051, .T. ) ;
#3809 = ORIENTED_EDGE ( 'NONE', *, *, #9522, .T. ) ;
#3810 = FILL_AREA_STYLE ('',( #12321 ) ) ;
#3811 = ORIENTED_EDGE ( 'NONE', *, *, #1313, .T. ) ;
#3812 = ADVANCED_FACE ( 'NONE', ( #7768 ), #1720, .T. ) ;
#3813 = FACE_OUTER_BOUND ( 'NONE', #788, .T. ) ;
#3814 = VECTOR ( 'NONE', #7172, 1000.000000000000000 ) ;
#3815 = DIRECTION ( 'NONE',  ( -1.000000000000000000, -0.000000000000000000, 0.000000000000000000 ) ) ;
#3816 = EDGE_LOOP ( 'NONE', ( #4703, #15598 ) ) ;
#3817 = VERTEX_POINT ( 'NONE', #391 ) ;
#3818 = CARTESIAN_POINT ( 'NONE',  ( -186.0388298304660282, 135.7737150272329529, -2.963320117457103109 ) ) ;
#3819 = CARTESIAN_POINT ( 'NONE',  ( 191.4249991583111523, 42.11970308376083949, -6.062475933048471433 ) ) ;
#3820 = EDGE_CURVE ( 'NONE', #1161, #3061, #1516, .T. ) ;
#3821 = ORIENTED_EDGE ( 'NONE', *, *, #14885, .F. ) ;
#3822 = DIRECTION ( 'NONE',  ( 1.000000000000000000, -2.751328491981765035E-32, 3.965082230804130220E-16 ) ) ;
#3823 = CARTESIAN_POINT ( 'NONE',  ( -164.5262273476080850, 106.7842295329139262, 5.000000000000000000 ) ) ;
#3824 = EDGE_CURVE ( 'NONE', #8794, #944, #13667, .T. ) ;
#3825 = EDGE_CURVE ( 'NONE', #13113, #15168, #5230, .T. ) ;
#3826 = LINE ( 'NONE', #8646, #11079 ) ;
#3827 = CIRCLE ( 'NONE', #12885, 380.9270036976043343 ) ;
#3828 = CIRCLE ( 'NONE', #3076, 0.5000000000000000000 ) ;
#3829 = VERTEX_POINT ( 'NONE', #1749 ) ;
#3830 = CARTESIAN_POINT ( 'NONE',  ( -76.00000000000001421, -178.8058001507315566, 52.69066787724494816 ) ) ;
#3831 = CARTESIAN_POINT ( 'NONE',  ( 193.0763172156907501, 35.56634871065938341, -4.111983000380113218 ) ) ;
#3832 = VERTEX_POINT ( 'NONE', #11307 ) ;
#3833 = CARTESIAN_POINT ( 'NONE',  ( -157.8787660911425803, 118.6941998492684149, 5.000000000000000000 ) ) ;
#3834 = CARTESIAN_POINT ( 'NONE',  ( -35.99999999999995026, 62.13993994372673768, 13.30000000000139870 ) ) ;
#3835 = CARTESIAN_POINT ( 'NONE',  ( -178.4226240946890130, 124.9752285324798606, -5.265047855996060733 ) ) ;
#3836 = EDGE_LOOP ( 'NONE', ( #12094, #10696 ) ) ;
#3837 = CARTESIAN_POINT ( 'NONE',  ( -204.9546745879972889, 133.0893851581147374, 7.918248976830629893 ) ) ;
#3839 = CARTESIAN_POINT ( 'NONE',  ( 208.7932886394164598, 39.56360219514107257, 0.008477354278063056400 ) ) ;
#3838 = CIRCLE ( 'NONE', #5853, 1.000000000000000888 ) ;
#3840 = EDGE_CURVE ( 'NONE', #12019, #3756, #468, .T. ) ;
#3841 = EDGE_CURVE ( 'NONE', #14207, #13704, #11817, .T. ) ;
#3842 = ORIENTED_EDGE ( 'NONE', *, *, #11844, .F. ) ;
#3843 = EDGE_CURVE ( 'NONE', #9433, #645, #4118, .T. ) ;
#3844 = ORIENTED_EDGE ( 'NONE', *, *, #9771, .F. ) ;
#3845 = AXIS2_PLACEMENT_3D ( 'NONE', #5679, #3460, #7106 ) ;
#3846 = CARTESIAN_POINT ( 'NONE',  ( 0.7145311798163189732, 4.618802153516981868, 8.000000000000007105 ) ) ;
#3847 = CARTESIAN_POINT ( 'NONE',  ( -156.6477983077465410, 110.1970436846185066, 5.000000000000000000 ) ) ;
#3848 = CARTESIAN_POINT ( 'NONE',  ( 6.399999999999999467, -4.618802153517037823, -7.999999999999979572 ) ) ;
#3849 = DIRECTION ( 'NONE',  ( 0.000000000000000000, -0.9902680687415712502, -0.1391731009600586100 ) ) ;
#3850 = AXIS2_PLACEMENT_3D ( 'NONE', #11150, #2857, #302 ) ;
#3851 = FACE_OUTER_BOUND ( 'NONE', #5147, .T. ) ;
#3852 = EDGE_CURVE ( 'NONE', #10197, #13912, #236, .T. ) ;
#3853 = CARTESIAN_POINT ( 'NONE',  ( -188.8176989649505231, 137.2180184133358694, 7.919662025281898998 ) ) ;
#3854 = CARTESIAN_POINT ( 'NONE',  ( -76.00000000000004263, -179.3058001507315566, 64.88378295107887084 ) ) ;
#3855 = CARTESIAN_POINT ( 'NONE',  ( -150.4086188282879277, 107.2728346664360259, 84.88378295107887084 ) ) ;
#3856 = ORIENTED_EDGE ( 'NONE', *, *, #11167, .F. ) ;
#3857 = DIRECTION ( 'NONE',  ( 0.000000000000000000, -0.1391731009600641333, -0.9902680687415704730 ) ) ;
#3858 = ORIENTED_EDGE ( 'NONE', *, *, #3841, .F. ) ;
#3859 = DIRECTION ( 'NONE',  ( 1.000000000000000000, 0.000000000000000000, 0.000000000000000000 ) ) ;
#3860 = CYLINDRICAL_SURFACE ( 'NONE', #10644, 1.499999999999995115 ) ;
#3861 = CARTESIAN_POINT ( 'NONE',  ( 164.0000000000000568, 64.53993994372673626, 15.00000000000000355 ) ) ;
#3862 = CARTESIAN_POINT ( 'NONE',  ( -76.00000000000001421, 15.03993994372673981, -3.075184203610571654 ) ) ;
#3863 = CARTESIAN_POINT ( 'NONE',  ( -88.77455057502459113, 65.19100426474074084, 10.00000000000000178 ) ) ;
#3864 = CARTESIAN_POINT ( 'NONE',  ( -207.9892458934089632, 147.4169567187306029, 7.919662025281897222 ) ) ;
#3865 = ORIENTED_EDGE ( 'NONE', *, *, #1797, .T. ) ;
#3866 = CIRCLE ( 'NONE', #12673, 0.5000000000000004441 ) ;
#3867 = EDGE_CURVE ( 'NONE', #8197, #3324, #8716, .T. ) ;
#3868 = CARTESIAN_POINT ( 'NONE',  ( 0.02377086945385613326, 0.5410735902593410973, -2.749999999999999112 ) ) ;
#3869 = CARTESIAN_POINT ( 'NONE',  ( -222.2279178565764255, 149.0830140542140043, 7.930883854505606401 ) ) ;
#3870 = ORIENTED_EDGE ( 'NONE', *, *, #8268, .F. ) ;
#3871 = AXIS2_PLACEMENT_3D ( 'NONE', #8447, #15514, #3536 ) ;
#3872 = CARTESIAN_POINT ( 'NONE',  ( -220.1006191622630297, 148.8276055330639736, 9.939501965825337848 ) ) ;
#3873 = EDGE_LOOP ( 'NONE', ( #11108, #14364, #10374, #5700 ) ) ;
#3874 = CARTESIAN_POINT ( 'NONE',  ( -173.8777679508388019, 116.7033564454829673, -1.424210617517640554 ) ) ;
#3875 = CARTESIAN_POINT ( 'NONE',  ( 198.5010533697851827, 29.08139766703656903, -5.315318924259303301 ) ) ;
#3877 = EDGE_LOOP ( 'NONE', ( #1117, #14798 ) ) ;
#3876 = VECTOR ( 'NONE', #9303, 1000.000000000000000 ) ;
#3878 = DIRECTION ( 'NONE',  ( 0.000000000000000000, -0.9902680687415712502, -0.1391731009600596092 ) ) ;
#3879 = DIRECTION ( 'NONE',  ( 0.000000000000000000, 0.000000000000000000, 1.000000000000000000 ) ) ;
#3880 = EDGE_CURVE ( 'NONE', #14252, #2155, #2792, .T. ) ;
#3881 = DIRECTION ( 'NONE',  ( 0.000000000000000000, 2.731481088613025116E-16, -1.000000000000000000 ) ) ;
#3882 = EDGE_LOOP ( 'NONE', ( #5039, #5265 ) ) ;
#3883 = AXIS2_PLACEMENT_3D ( 'NONE', #5256, #13696, #2900 ) ;
#3884 = DIRECTION ( 'NONE',  ( 1.000000000000000000, 0.000000000000000000, 0.000000000000000000 ) ) ;
#3885 = ORIENTED_EDGE ( 'NONE', *, *, #13530, .F. ) ;
#3886 = CIRCLE ( 'NONE', #840, 1.000000000000000888 ) ;
#3887 = CARTESIAN_POINT ( 'NONE',  ( -76.00000000000001421, 15.53993994372673981, 10.05257423913146475 ) ) ;
#3888 = ORIENTED_EDGE ( 'NONE', *, *, #3383, .F. ) ;
#3889 = FACE_BOUND ( 'NONE', #15005, .T. ) ;
#3890 = CARTESIAN_POINT ( 'NONE',  ( 184.0000000000000568, -181.3058001507315566, 77.95141194869098911 ) ) ;
#3891 = ORIENTED_EDGE ( 'NONE', *, *, #1198, .T. ) ;
#3892 = ORIENTED_EDGE ( 'NONE', *, *, #5465, .F. ) ;
#3893 = DIRECTION ( 'NONE',  ( -1.000000000000000000, 0.000000000000000000, 0.000000000000000000 ) ) ;
#3894 = EDGE_CURVE ( 'NONE', #5784, #10772, #9051, .T. ) ;
#3895 = CARTESIAN_POINT ( 'NONE',  ( 0.000000000000000000, 0.000000000000000000, 0.000000000000000000 ) ) ;
#3896 = AXIS2_PLACEMENT_3D ( 'NONE', #4839, #6186, #9813 ) ;
#3897 = ORIENTED_EDGE ( 'NONE', *, *, #4291, .T. ) ;
#3898 = CARTESIAN_POINT ( 'NONE',  ( -64.00000000000002842, -178.9449732516916072, -29.32815825124560760 ) ) ;
#3899 = LINE ( 'NONE', #9828, #3926 ) ;
#3900 = FACE_OUTER_BOUND ( 'NONE', #3960, .T. ) ;
#3901 = ADVANCED_FACE ( 'NONE', ( #12790 ), #14055, .T. ) ;
#3902 = CARTESIAN_POINT ( 'NONE',  ( 203.7958462291278749, 29.94547861640233322, -6.526400227122580944 ) ) ;
#3903 = ORIENTED_EDGE ( 'NONE', *, *, #14111, .T. ) ;
#3904 = CARTESIAN_POINT ( 'NONE',  ( 114.0000000000000568, 64.51493994372674479, 18.50000000000035527 ) ) ;
#3905 = CARTESIAN_POINT ( 'NONE',  ( -222.7490783815899533, 143.6991938219488247, -2.614991558308088937 ) ) ;
#3906 = CARTESIAN_POINT ( 'NONE',  ( -214.7080733591933779, 145.5905563435376848, -5.230826428279589990 ) ) ;
#3907 = DIRECTION ( 'NONE',  ( 0.000000000000000000, 0.7071067811865474617, 0.7071067811865474617 ) ) ;
#3908 = ORIENTED_EDGE ( 'NONE', *, *, #17, .T. ) ;
#3909 = CARTESIAN_POINT ( 'NONE',  ( -168.3973611425364822, 125.8284172634911755, 7.880738923213935543 ) ) ;
#3910 = CARTESIAN_POINT ( 'NONE',  ( 205.4107168461011099, 33.83372868983673243, -6.361989640121679557 ) ) ;
#3911 = ORIENTED_EDGE ( 'NONE', *, *, #2206, .F. ) ;
#3912 = ORIENTED_EDGE ( 'NONE', *, *, #13958, .T. ) ;
#3913 = AXIS2_PLACEMENT_3D ( 'NONE', #12727, #11403, #569 ) ;
#3914 = DIRECTION ( 'NONE',  ( -1.000000000000000000, 0.000000000000000000, -0.000000000000000000 ) ) ;
#3915 = FACE_OUTER_BOUND ( 'NONE', #8848, .T. ) ;
#3916 = CARTESIAN_POINT ( 'NONE',  ( 51.39999999999999858, 0.000000000000000000, 0.000000000000000000 ) ) ;
#3917 = ADVANCED_FACE ( 'NONE', ( #4426 ), #6670, .T. ) ;
#3918 = CARTESIAN_POINT ( 'NONE',  ( -63.50000000000002842, 17.53993994372674692, -17.50000000000002487 ) ) ;
#3920 = EDGE_CURVE ( 'NONE', #8640, #4430, #13567, .T. ) ;
#3919 = EDGE_CURVE ( 'NONE', #6568, #13786, #11566, .T. ) ;
#3921 = DIRECTION ( 'NONE',  ( 1.000000000000000000, 0.000000000000000000, 3.965082230804112963E-16 ) ) ;
#3922 = CARTESIAN_POINT ( 'NONE',  ( -167.6801169734147265, 127.1165587117766336, 5.426559898713293251 ) ) ;
#3923 = LINE ( 'NONE', #116, #13312 ) ;
#3924 = LINE ( 'NONE', #9863, #9146 ) ;
#3925 = ORIENTED_EDGE ( 'NONE', *, *, #10114, .T. ) ;
#3926 = VECTOR ( 'NONE', #12256, 1000.000000000000000 ) ;
#3927 = DIRECTION ( 'NONE',  ( 5.518327896226373923E-17, -0.9902680687415712502, -0.1391731009600586100 ) ) ;
#3928 = EDGE_LOOP ( 'NONE', ( #7060, #121, #6529, #3566 ) ) ;
#3929 = ORIENTED_EDGE ( 'NONE', *, *, #5008, .T. ) ;
#3930 = CARTESIAN_POINT ( 'NONE',  ( -151.5638213263409853, 108.2696846136310711, 9.788006227097797662 ) ) ;
#3931 = CARTESIAN_POINT ( 'NONE',  ( 203.0705284447388124, 48.84127762431399589, -0.9107274384406883749 ) ) ;
#3932 = FACE_OUTER_BOUND ( 'NONE', #4207, .T. ) ;
#3933 = DIRECTION ( 'NONE',  ( 0.000000000000000000, -5.551115123125765446E-17, 1.000000000000000000 ) ) ;
#3934 = DIRECTION ( 'NONE',  ( -1.000000000000000000, 0.000000000000000000, 0.000000000000000000 ) ) ;
#3935 = CARTESIAN_POINT ( 'NONE',  ( 0.2456200930617507272, -1.587713240271640958, -2.750000000000000888 ) ) ;
#3936 = CARTESIAN_POINT ( 'NONE',  ( -211.4864660300886499, 151.5260579444296525, 5.434754235172608361 ) ) ;
#3937 = AXIS2_PLACEMENT_3D ( 'NONE', #7862, #1834, #11547 ) ;
#3938 = VERTEX_POINT ( 'NONE', #6741 ) ;
#3939 = AXIS2_PLACEMENT_3D ( 'NONE', #8815, #13691, #8739 ) ;
#3940 = DIRECTION ( 'NONE',  ( 0.000000000000000000, 1.000000000000000000, 6.938893903907227145E-17 ) ) ;
#3941 = PRODUCT_DEFINITION_CONTEXT ( 'detailed design', #11595, 'design' ) ;
#3942 = CARTESIAN_POINT ( 'NONE',  ( 201.3402840685550643, 32.17245832385849980, -2.180909807981465054 ) ) ;
#3943 = CARTESIAN_POINT ( 'NONE',  ( -222.4836136237429116, 148.6248949498702530, 7.868731570916820850 ) ) ;
#3944 = ORIENTED_EDGE ( 'NONE', *, *, #5654, .F. ) ;
#3945 = CARTESIAN_POINT ( 'NONE',  ( -220.2521499497359230, 152.6229124025628323, 6.494025194934711642 ) ) ;
#3946 = VERTEX_POINT ( 'NONE', #5702 ) ;
#3947 = CARTESIAN_POINT ( 'NONE',  ( -35.99999999999995026, 62.13993994372673768, 11.50000000000139622 ) ) ;
#3948 = DIRECTION ( 'NONE',  ( 1.000000000000000000, 0.000000000000000000, 0.000000000000000000 ) ) ;
#3949 = VERTEX_POINT ( 'NONE', #5474 ) ;
#3950 = FACE_OUTER_BOUND ( 'NONE', #5492, .T. ) ;
#3951 = CARTESIAN_POINT ( 'NONE',  ( 0.3167204509598258722, 8.479269695850844002, -1.313474075707198097 ) ) ;
#3952 = EDGE_CURVE ( 'NONE', #9376, #7692, #15563, .T. ) ;
#3953 = DIRECTION ( 'NONE',  ( 0.000000000000000000, -0.1391731009600660485, -0.9902680687415702510 ) ) ;
#3954 = ORIENTED_EDGE ( 'NONE', *, *, #12381, .F. ) ;
#3955 = VERTEX_POINT ( 'NONE', #8089 ) ;
#3956 = CARTESIAN_POINT ( 'NONE',  ( -157.1737171244663784, 111.0576063001072953, 9.722517344254139715 ) ) ;
#3957 = EDGE_LOOP ( 'NONE', ( #7121, #9893, #6894, #14139 ) ) ;
#3958 = DIRECTION ( 'NONE',  ( 0.000000000000000000, 0.000000000000000000, -1.000000000000000000 ) ) ;
#3959 = PLANE ( 'NONE',  #3761 ) ;
#3960 = EDGE_LOOP ( 'NONE', ( #15052, #9761, #3641, #10584 ) ) ;
#3961 = EDGE_LOOP ( 'NONE', ( #8239, #8863 ) ) ;
#3962 = DIRECTION ( 'NONE',  ( -0.000000000000000000, 0.000000000000000000, 1.000000000000000000 ) ) ;
#3963 = CARTESIAN_POINT ( 'NONE',  ( 201.3402840685550643, 32.17245832385849980, -2.180909807981465054 ) ) ;
#3964 = ORIENTED_EDGE ( 'NONE', *, *, #3183, .T. ) ;
#3965 = EDGE_CURVE ( 'NONE', #6346, #9678, #9263, .T. ) ;
#3966 = CARTESIAN_POINT ( 'NONE',  ( -155.6477983077466263, 110.0646653313681043, -4.828669606760402466 ) ) ;
#3967 = CARTESIAN_POINT ( 'NONE',  ( -63.50000000000002842, -179.8058001507315566, 65.31842631998698323 ) ) ;
#3968 = CYLINDRICAL_SURFACE ( 'NONE', #14362, 1.699999999999993072 ) ;
#3969 = CARTESIAN_POINT ( 'NONE',  ( 51.07686401294030532, 368.7106150007013525, 10.00000000000000178 ) ) ;
#3970 = ORIENTED_EDGE ( 'NONE', *, *, #2284, .T. ) ;
#3971 =( NAMED_UNIT ( * ) PLANE_ANGLE_UNIT ( ) SI_UNIT ( $, .RADIAN. ) );
#3972 = CARTESIAN_POINT ( 'NONE',  ( -219.1618877908461513, 150.5179266800831215, -4.694150837216314542 ) ) ;
#3973 = AXIS2_PLACEMENT_3D ( 'NONE', #2941, #4112, #3016 ) ;
#3974 = CARTESIAN_POINT ( 'NONE',  ( -197.2022238459480263, 131.7665462075744358, -4.642206099735013858 ) ) ;
#3975 = DIRECTION ( 'NONE',  ( 1.000000000000000000, 0.000000000000000000, 0.000000000000000000 ) ) ;
#3976 = ORIENTED_EDGE ( 'NONE', *, *, #2174, .T. ) ;
#3977 = CARTESIAN_POINT ( 'NONE',  ( -205.7735142771631160, 131.5899501701119334, 5.434137442415934771 ) ) ;
#3978 = CARTESIAN_POINT ( 'NONE',  ( 193.0763172156907501, 35.56634871065938341, -4.111983000380113218 ) ) ;
#3979 = VERTEX_POINT ( 'NONE', #10281 ) ;
#3980 = ORIENTED_EDGE ( 'NONE', *, *, #4833, .T. ) ;
#3981 = EDGE_CURVE ( 'NONE', #2293, #1098, #10515, .T. ) ;
#3982 = DIRECTION ( 'NONE',  ( -0.000000000000000000, 1.000000000000000000, 6.938893903907227145E-17 ) ) ;
#3983 = PLANE ( 'NONE',  #6478 ) ;
#3984 = DIRECTION ( 'NONE',  ( -0.1562424607007877608, 0.2866315678550999668, -0.9452145987991775744 ) ) ;
#3985 = VECTOR ( 'NONE', #11034, 1000.000000000000000 ) ;
#3986 = DIRECTION ( 'NONE',  ( -0.000000000000000000, -0.000000000000000000, -1.000000000000000000 ) ) ;
#3987 = CARTESIAN_POINT ( 'NONE',  ( -10.39230484541326582, 4.570335331080236228E-16, 5.000000000000000000 ) ) ;
#3988 = VECTOR ( 'NONE', #9491, 1000.000000000000000 ) ;
#3989 = CARTESIAN_POINT ( 'NONE',  ( -193.7244371550166022, 142.0541455854551600, 3.478855109513427468 ) ) ;
#3990 = CIRCLE ( 'NONE', #12816, 1.699999999999991518 ) ;
#3991 = PLANE ( 'NONE',  #11807 ) ;
#3992 = DIRECTION ( 'NONE',  ( 0.000000000000000000, 1.000000000000000000, 6.938893903907222067E-15 ) ) ;
#3993 = ORIENTED_EDGE ( 'NONE', *, *, #13266, .F. ) ;
#3994 = EDGE_CURVE ( 'NONE', #10853, #5266, #6774, .T. ) ;
#3995 = DIRECTION ( 'NONE',  ( -0.000000000000000000, -0.000000000000000000, 1.000000000000000000 ) ) ;
#3996 = CIRCLE ( 'NONE', #12819, 17.06579782980005433 ) ;
#3997 = VERTEX_POINT ( 'NONE', #15307 ) ;
#3998 = ORIENTED_EDGE ( 'NONE', *, *, #625, .F. ) ;
#3999 = CARTESIAN_POINT ( 'NONE',  ( 190.5000000000000568, 17.53993994372674692, -17.50000000000002487 ) ) ;
#4000 = CARTESIAN_POINT ( 'NONE',  ( -136.1405586187959784, 108.3975249866138597, 0.000000000000000000 ) ) ;
#4001 = CARTESIAN_POINT ( 'NONE',  ( -70.00000000000000000, -181.3058001507315566, 76.45141194869098911 ) ) ;
#4002 = LINE ( 'NONE', #7579, #10686 ) ;
#4003 = CARTESIAN_POINT ( 'NONE',  ( -108.0000000000000568, 59.53993994372674337, 10.00000000000000178 ) ) ;
#4004 = EDGE_CURVE ( 'NONE', #8914, #810, #8244, .T. ) ;
#4005 = CARTESIAN_POINT ( 'NONE',  ( -219.4404776672114963, 154.0771507077609499, 1.641297965848094842 ) ) ;
#4006 = CARTESIAN_POINT ( 'NONE',  ( -170.1156333370428229, 128.4548013739684791, 5.428578397873499384 ) ) ;
#4007 = AXIS2_PLACEMENT_3D ( 'NONE', #7699, #5082, #475 ) ;
#4008 = EDGE_CURVE ( 'NONE', #5990, #3704, #8784, .T. ) ;
#4009 = ORIENTED_EDGE ( 'NONE', *, *, #3337, .T. ) ;
#4010 = CIRCLE ( 'NONE', #3009, 0.5000000000000004441 ) ;
#4011 = CARTESIAN_POINT ( 'NONE',  ( -1.350735206554858068E-15, 2.246824879981693890, -1.608385152161860399 ) ) ;
#4012 = CARTESIAN_POINT ( 'NONE',  ( 191.4249991583111523, 42.11970308376083949, -6.062475933048471433 ) ) ;
#4013 = CARTESIAN_POINT ( 'NONE',  ( -34.79899788034579444, 48.72489408690345414, 9.975000000000001421 ) ) ;
#4014 = ORIENTED_EDGE ( 'NONE', *, *, #2769, .T. ) ;
#4015 = AXIS2_PLACEMENT_3D ( 'NONE', #957, #4751, #8252 ) ;
#4016 = AXIS2_PLACEMENT_3D ( 'NONE', #10978, #4896, #13243 ) ;
#4017 = CARTESIAN_POINT ( 'NONE',  ( -222.1940576498694213, 149.1436799296412801, 9.935665413336629115 ) ) ;
#4018 = ORIENTED_EDGE ( 'NONE', *, *, #9853, .F. ) ;
#4019 = CARTESIAN_POINT ( 'NONE',  ( -168.5042799224661110, 126.3308037436463849, -2.295422687810467099 ) ) ;
#4020 = DIRECTION ( 'NONE',  ( 0.000000000000000000, -1.000000000000000000, 0.000000000000000000 ) ) ;
#4021 = EDGE_CURVE ( 'NONE', #5329, #8949, #1978, .T. ) ;
#4022 = EDGE_LOOP ( 'NONE', ( #6936, #12113, #4860, #6629 ) ) ;
#4024 = EDGE_CURVE ( 'NONE', #5590, #10586, #7289, .T. ) ;
#4023 =( REPRESENTATION_RELATIONSHIP ('NONE','NONE', #3298, #10258 ) REPRESENTATION_RELATIONSHIP_WITH_TRANSFORMATION ( #11381 )SHAPE_REPRESENTATION_RELATIONSHIP( ) );
#4025 = CARTESIAN_POINT ( 'NONE',  ( 167.9295236634097819, 65.51901744756737855, -0.9107274384406879308 ) ) ;
#4026 = CARTESIAN_POINT ( 'NONE',  ( 190.0000000000000568, 11.87216911405867670, 8.597545510065431884 ) ) ;
#4027 = CARTESIAN_POINT ( 'NONE',  ( 177.5000000000000853, 19.53993994372674692, -17.50000000000002487 ) ) ;
#4028 = VERTEX_POINT ( 'NONE', #703 ) ;
#4029 = TOROIDAL_SURFACE ( 'NONE', #5564, 1.000000000000000000, 0.5000000000000000000 ) ;
#4030 = DIRECTION ( 'NONE',  ( 0.000000000000000000, 0.000000000000000000, -1.000000000000000000 ) ) ;
#4031 = ORIENTED_EDGE ( 'NONE', *, *, #8964, .F. ) ;
#4032 = LINE ( 'NONE', #2863, #9200 ) ;
#4033 = DIRECTION ( 'NONE',  ( 0.000000000000000000, 0.000000000000000000, 1.000000000000000000 ) ) ;
#4034 = EDGE_LOOP ( 'NONE', ( #10441, #8376 ) ) ;
#4035 = DIRECTION ( 'NONE',  ( -0.4873681696970824651, -0.8731965799097680669, 0.000000000000000000 ) ) ;
#4036 = ADVANCED_FACE ( 'NONE', ( #11628 ), #15390, .F. ) ;
#4037 = DIRECTION ( 'NONE',  ( 0.000000000000000000, 0.000000000000000000, 1.000000000000000000 ) ) ;
#4038 = ORIENTED_EDGE ( 'NONE', *, *, #4337, .T. ) ;
#4039 = EDGE_LOOP ( 'NONE', ( #10951, #8463 ) ) ;
#4040 = CARTESIAN_POINT ( 'NONE',  ( -187.9132138465967898, 138.8208849330412988, 2.500000000000000000 ) ) ;
#4041 = CARTESIAN_POINT ( 'NONE',  ( -5.000000000000000000, 0.000000000000000000, 5.000000000000000000 ) ) ;
#4042 = CIRCLE ( 'NONE', #762, 1.700000000000007061 ) ;
#4043 = EDGE_LOOP ( 'NONE', ( #6956, #15068, #3151, #3747, #7627, #11912 ) ) ;
#4044 = CARTESIAN_POINT ( 'NONE',  ( 198.8872864542346974, 32.16591232847088122, -2.310211674251309688 ) ) ;
#4045 = DIRECTION ( 'NONE',  ( 0.7071067811864983899, 0.000000000000000000, 0.7071067811865966446 ) ) ;
#4046 = FACE_OUTER_BOUND ( 'NONE', #9753, .T. ) ;
#4047 = CARTESIAN_POINT ( 'NONE',  ( -110.0000000000000426, 19.53993994372674337, 24.99999999999999645 ) ) ;
#4048 = DIRECTION ( 'NONE',  ( 0.000000000000000000, -1.000000000000000000, 0.000000000000000000 ) ) ;
#4049 = VECTOR ( 'NONE', #7915, 1000.000000000000000 ) ;
#4050 = AXIS2_PLACEMENT_3D ( 'NONE', #7134, #2219, #8473 ) ;
#4051 = PRESENTATION_STYLE_ASSIGNMENT (( #11173 ) ) ;
#4052 = EDGE_CURVE ( 'NONE', #15155, #8082, #15316, .T. ) ;
#4053 = VERTEX_POINT ( 'NONE', #13910 ) ;
#4054 = LINE ( 'NONE', #11248, #14897 ) ;
#4055 = CARTESIAN_POINT ( 'NONE',  ( -216.7768923448186342, 154.7526869307816071, 0.8713118593939417345 ) ) ;
#4056 = CARTESIAN_POINT ( 'NONE',  ( -220.6443225159919734, 151.9202736894074803, -4.662307221713795968 ) ) ;
#4057 = CARTESIAN_POINT ( 'NONE',  ( -76.50000000000004263, 15.53993994372673626, 52.49999999999997868 ) ) ;
#4058 = VERTEX_POINT ( 'NONE', #8006 ) ;
#4059 = CARTESIAN_POINT ( 'NONE',  ( -176.4886329031608909, 117.0201139606268441, 5.242686462712208062 ) ) ;
#4060 = UNCERTAINTY_MEASURE_WITH_UNIT (LENGTH_MEASURE( 1.000000000000000082E-05 ), #12452, 'distance_accuracy_value', 'NONE');
#4061 = CARTESIAN_POINT ( 'NONE',  ( 198.8102040144913758, 32.17279782253822162, -0.7412068558913099681 ) ) ;
#4062 = VERTEX_POINT ( 'NONE', #3102 ) ;
#4063 = VECTOR ( 'NONE', #15308, 1000.000000000000000 ) ;
#4064 = DIRECTION ( 'NONE',  ( 1.000000000000000000, 0.000000000000000000, 0.000000000000000000 ) ) ;
#4065 = CARTESIAN_POINT ( 'NONE',  ( 184.0000000000000568, 15.53993994372673981, -10.99999999999999645 ) ) ;
#4066 = AXIS2_PLACEMENT_3D ( 'NONE', #8081, #14859, #12866 ) ;
#4067 = DIRECTION ( 'NONE',  ( 0.000000000000000000, 0.000000000000000000, 1.000000000000000000 ) ) ;
#4068 = EDGE_CURVE ( 'NONE', #4062, #10761, #6814, .T. ) ;
#4069 = CARTESIAN_POINT ( 'NONE',  ( -61.94838851346079167, -179.3058001507315566, -17.76585208085566947 ) ) ;
#4070 = VERTEX_POINT ( 'NONE', #13100 ) ;
#4071 = VECTOR ( 'NONE', #12530, 1000.000000000000000 ) ;
#4072 = CYLINDRICAL_SURFACE ( 'NONE', #606, 3.500000000000003109 ) ;
#4073 = CARTESIAN_POINT ( 'NONE',  ( -170.1156333370428229, 128.4548013739684791, 5.428578397873499384 ) ) ;
#4074 = CYLINDRICAL_SURFACE ( 'NONE', #5253, 1.499999999999997780 ) ;
#4075 = CIRCLE ( 'NONE', #11906, 1.500000000000001332 ) ;
#4076 = CARTESIAN_POINT ( 'NONE',  ( 6.399999999999999467, 9.797174393178827630E-16, -8.000000000000000000 ) ) ;
#4077 = ORIENTED_EDGE ( 'NONE', *, *, #1422, .F. ) ;
#4078 = EDGE_CURVE ( 'NONE', #5262, #6618, #8618, .T. ) ;
#4079 = CARTESIAN_POINT ( 'NONE',  ( -64.00000000000002842, 15.53993994372673804, 24.94742576086838781 ) ) ;
#4080 = ORIENTED_EDGE ( 'NONE', *, *, #8736, .T. ) ;
#4081 = ORIENTED_EDGE ( 'NONE', *, *, #15451, .T. ) ;
#4082 = CARTESIAN_POINT ( 'NONE',  ( -85.99999999999994316, 64.53993994372673626, 15.00000000000174794 ) ) ;
#4083 = DIRECTION ( 'NONE',  ( 1.000000000000000000, 0.000000000000000000, 0.000000000000000000 ) ) ;
#4084 = EDGE_CURVE ( 'NONE', #12187, #5228, #3639, .T. ) ;
#4085 = DIRECTION ( 'NONE',  ( 0.000000000000000000, 0.000000000000000000, -1.000000000000000000 ) ) ;
#4086 = CARTESIAN_POINT ( 'NONE',  ( -160.1026119161506358, 114.7098309688581708, 2.431557144026069928 ) ) ;
#4087 = CARTESIAN_POINT ( 'NONE',  ( 193.1062858801516882, 40.86394065090267702, 16.00000000000001421 ) ) ;
#4088 = VECTOR ( 'NONE', #4540, 1000.000000000000000 ) ;
#4089 = CARTESIAN_POINT ( 'NONE',  ( -218.3154676233766338, 152.0521266355204091, -3.827015397074207570 ) ) ;
#4090 = COLOUR_RGB ( '', 0.66274510, 0.83137255, 0.94901961) ;
#4091 = EDGE_LOOP ( 'NONE', ( #15037, #1289, #793, #15522 ) ) ;
#4092 = LINE ( 'NONE', #7825, #9192 ) ;
#4093 = EDGE_CURVE ( 'NONE', #13859, #12311, #12012, .T. ) ;
#4094 = LINE ( 'NONE', #5207, #5339 ) ;
#4095 = CARTESIAN_POINT ( 'NONE',  ( -221.8782673190674188, 149.7094678780368042, -3.059957786096294097 ) ) ;
#4096 = VERTEX_POINT ( 'NONE', #13332 ) ;
#4097 = CARTESIAN_POINT ( 'NONE',  ( -218.8494421554486848, 151.1141414623175763, 9.296710778528519015 ) ) ;
#4098 = ORIENTED_EDGE ( 'NONE', *, *, #436, .F. ) ;
#4099 = CYLINDRICAL_SURFACE ( 'NONE', #453, 1.699999999999993072 ) ;
#4100 = DIRECTION ( 'NONE',  ( 0.000000000000000000, 0.000000000000000000, 1.000000000000000000 ) ) ;
#4101 = ORIENTED_EDGE ( 'NONE', *, *, #14410, .T. ) ;
#4102 = CARTESIAN_POINT ( 'NONE',  ( 205.1062858801516597, 40.86394065090267702, -219.0000000000000853 ) ) ;
#4103 = DIRECTION ( 'NONE',  ( -0.000000000000000000, -0.000000000000000000, 1.000000000000000000 ) ) ;
#4104 = PRODUCT_DEFINITION_SHAPE ( 'NONE', 'NONE',  #12882 ) ;
#4105 = AXIS2_PLACEMENT_3D ( 'NONE', #6100, #13257, #3715 ) ;
#4106 = DIRECTION ( 'NONE',  ( 0.000000000000000000, 1.000000000000000000, 2.731481088613025116E-16 ) ) ;
#4107 = ORIENTED_EDGE ( 'NONE', *, *, #1778, .T. ) ;
#4108 = EDGE_LOOP ( 'NONE', ( #9068, #2784, #315, #15001 ) ) ;
#4109 = ADVANCED_FACE ( 'NONE', ( #2452 ), #8402, .F. ) ;
#4110 = ADVANCED_FACE ( 'NONE', ( #5859 ), #10752, .F. ) ;
#4111 = EDGE_CURVE ( 'NONE', #10853, #8004, #4740, .T. ) ;
#4112 = DIRECTION ( 'NONE',  ( 1.000000000000000000, 2.751328491981765035E-32, -3.965082230804130220E-16 ) ) ;
#4113 = ORIENTED_EDGE ( 'NONE', *, *, #5152, .F. ) ;
#4114 = CARTESIAN_POINT ( 'NONE',  ( 205.1062858801516597, 40.86394065090267702, 5.000000000000000000 ) ) ;
#4115 = DIRECTION ( 'NONE',  ( 0.000000000000000000, 0.000000000000000000, 1.000000000000000000 ) ) ;
#4116 = ORIENTED_EDGE ( 'NONE', *, *, #14690, .F. ) ;
#4117 = ORIENTED_EDGE ( 'NONE', *, *, #10392, .F. ) ;
#4118 = LINE ( 'NONE', #1827, #10308 ) ;
#4119 = DIRECTION ( 'NONE',  ( -0.000000000000000000, 1.000000000000000000, -0.000000000000000000 ) ) ;
#4120 = ORIENTED_EDGE ( 'NONE', *, *, #9571, .F. ) ;
#4121 = CARTESIAN_POINT ( 'NONE',  ( 208.8060099514817978, 42.07246638764446089, -7.432400171711813996 ) ) ;
#4122 = PLANE ( 'NONE',  #14857 ) ;
#4123 = AXIS2_PLACEMENT_3D ( 'NONE', #14874, #6458, #5106 ) ;
#4124 = DIRECTION ( 'NONE',  ( 0.000000000000000000, 0.9902680687415713612, -0.1391731009600582492 ) ) ;
#4125 = DIRECTION ( 'NONE',  ( -1.000000000000000000, 0.000000000000000000, 0.000000000000000000 ) ) ;
#4126 = DIRECTION ( 'NONE',  ( 0.000000000000000000, 1.000000000000000000, -0.000000000000000000 ) ) ;
#4127 = AXIS2_PLACEMENT_3D ( 'NONE', #5331, #10077, #14948 ) ;
#4128 = CARTESIAN_POINT ( 'NONE',  ( -35.99999999999995026, 59.53993994372674337, 15.00000000000139977 ) ) ;
#4129 = ORIENTED_EDGE ( 'NONE', *, *, #13754, .F. ) ;
#4130 = CARTESIAN_POINT ( 'NONE',  ( 190.5000000000000568, 17.53993994372673981, -17.50000000000002487 ) ) ;
#4131 = CARTESIAN_POINT ( 'NONE',  ( -172.5271923976867470, 129.8359673051191123, -0.4588839673349612291 ) ) ;
#4132 = DIRECTION ( 'NONE',  ( 1.000000000000000000, 0.000000000000000000, 0.000000000000000000 ) ) ;
#4133 = ORIENTED_EDGE ( 'NONE', *, *, #14190, .T. ) ;
#4134 = CARTESIAN_POINT ( 'NONE',  ( -199.4124801547868913, 127.6177204676982910, 3.478895870929493483 ) ) ;
#4135 = CARTESIAN_POINT ( 'NONE',  ( 207.1288103955774318, 46.12660085639766550, -4.186765234109192768 ) ) ;
#4136 = VECTOR ( 'NONE', #2455, 1000.000000000000000 ) ;
#4137 = ORIENTED_EDGE ( 'NONE', *, *, #2366, .F. ) ;
#4138 = CARTESIAN_POINT ( 'NONE',  ( -110.0000000000000426, 59.53993994372674337, 25.00000000000000000 ) ) ;
#4139 = DIRECTION ( 'NONE',  ( -0.000000000000000000, -0.000000000000000000, 1.000000000000000000 ) ) ;
#4140 = EDGE_CURVE ( 'NONE', #4254, #4264, #1108, .T. ) ;
#4141 = FACE_BOUND ( 'NONE', #3617, .T. ) ;
#4142 = EDGE_CURVE ( 'NONE', #6706, #10355, #12813, .T. ) ;
#4143 = DIRECTION ( 'NONE',  ( 0.000000000000000000, -1.486905836551548832E-16, 1.000000000000000000 ) ) ;
#4144 = ORIENTED_EDGE ( 'NONE', *, *, #5726, .F. ) ;
#4145 = DIRECTION ( 'NONE',  ( 0.000000000000000000, 0.000000000000000000, 1.000000000000000000 ) ) ;
#4146 = CARTESIAN_POINT ( 'NONE',  ( -194.7616377892423714, 140.1172406977107130, 7.919662025281898998 ) ) ;
#4147 = CARTESIAN_POINT ( 'NONE',  ( 184.0000000000000568, -179.3058001507315566, -41.45141194869120227 ) ) ;
#4148 = CARTESIAN_POINT ( 'NONE',  ( -156.9354057470242765, 111.1637277590593982, -4.906715952278847936 ) ) ;
#4149 = ORIENTED_EDGE ( 'NONE', *, *, #14811, .T. ) ;
#4150 = DIRECTION ( 'NONE',  ( 0.000000000000000000, 0.000000000000000000, -1.000000000000000000 ) ) ;
#4151 = CIRCLE ( 'NONE', #3410, 9.999999999999994671 ) ;
#4152 = VERTEX_POINT ( 'NONE', #3712 ) ;
#4153 = EDGE_LOOP ( 'NONE', ( #2579, #5385, #9025, #14054 ) ) ;
#4154 = LINE ( 'NONE', #7736, #15436 ) ;
#4155 = DIRECTION ( 'NONE',  ( 0.000000000000000000, -1.000000000000000000, 0.000000000000000000 ) ) ;
#4156 =( NAMED_UNIT ( * ) PLANE_ANGLE_UNIT ( ) SI_UNIT ( $, .RADIAN. ) );
#4157 = CARTESIAN_POINT ( 'NONE',  ( -220.3531759299249302, 148.3382346779569616, 2.431557144026069928 ) ) ;
#4158 = CARTESIAN_POINT ( 'NONE',  ( -218.4677351830677878, 155.8199715629169475, 3.280001329127711251 ) ) ;
#4159 = CARTESIAN_POINT ( 'NONE',  ( 200.1062858801516597, 40.86394065090267702, 12.00000000000001066 ) ) ;
#4160 = CIRCLE ( 'NONE', #7462, 1.000000000000000888 ) ;
#4161 = DIRECTION ( 'NONE',  ( -0.4873681696970814103, -0.8731965799097685110, -0.000000000000000000 ) ) ;
#4162 = CYLINDRICAL_SURFACE ( 'NONE', #7935, 1.700000000000007061 ) ;
#4163 = CIRCLE ( 'NONE', #7463, 0.4999999999999996114 ) ;
#4164 = EDGE_CURVE ( 'NONE', #10243, #5947, #10062, .T. ) ;
#4165 = CARTESIAN_POINT ( 'NONE',  ( 203.0658429208174880, 48.83360436048501896, -0.9158339742359169477 ) ) ;
#4166 = CARTESIAN_POINT ( 'NONE',  ( -219.4404776675327184, 154.0771507071854671, 1.641297965941626247 ) ) ;
#4167 = ORIENTED_EDGE ( 'NONE', *, *, #12126, .T. ) ;
#4168 = CARTESIAN_POINT ( 'NONE',  ( -219.1310489671168114, 154.6315407961138249, 6.827724881366695975 ) ) ;
#4169 = VERTEX_POINT ( 'NONE', #11859 ) ;
#4170 = CARTESIAN_POINT ( 'NONE',  ( -172.4948715304248594, 119.1810324607742615, -4.416274670461012519 ) ) ;
#4171 = DIRECTION ( 'NONE',  ( 0.000000000000000000, -1.000000000000000000, 0.000000000000000000 ) ) ;
#4172 = TOROIDAL_SURFACE ( 'NONE', #12243, 5.400000000000000355, 0.4000000000000000222 ) ;
#4173 = ORIENTED_EDGE ( 'NONE', *, *, #10294, .F. ) ;
#4174 = DIRECTION ( 'NONE',  ( -0.000000000000000000, -0.000000000000000000, -1.000000000000000000 ) ) ;
#4175 = DIRECTION ( 'NONE',  ( -1.000000000000000000, 0.000000000000000000, 0.000000000000000000 ) ) ;
#4176 = EDGE_CURVE ( 'NONE', #6305, #7344, #4909, .T. ) ;
#4177 = DIRECTION ( 'NONE',  ( -0.000000000000000000, -0.000000000000000000, 1.000000000000000000 ) ) ;
#4178 = ORIENTED_EDGE ( 'NONE', *, *, #14470, .T. ) ;
#4179 = APPLICATION_PROTOCOL_DEFINITION ( 'draft international standard', 'automotive_design', 1998, #1607 ) ;
#4180 = ORIENTED_EDGE ( 'NONE', *, *, #422, .F. ) ;
#4181 = CARTESIAN_POINT ( 'NONE',  ( 208.7932886394164598, 39.56360219514107257, 0.008477354278063056400 ) ) ;
#4182 = FACE_OUTER_BOUND ( 'NONE', #12272, .T. ) ;
#4183 = ORIENTED_EDGE ( 'NONE', *, *, #9927, .T. ) ;
#4184 = CARTESIAN_POINT ( 'NONE',  ( 177.5000000000000853, -178.8058001507315566, -17.19066787724516843 ) ) ;
#4185 = CARTESIAN_POINT ( 'NONE',  ( -151.4086188282879277, 107.2728346664360259, 0.000000000000000000 ) ) ;
#4186 = ORIENTED_EDGE ( 'NONE', *, *, #2371, .F. ) ;
#4187 = ORIENTED_EDGE ( 'NONE', *, *, #9421, .F. ) ;
#4188 = DIRECTION ( 'NONE',  ( 0.000000000000000000, -1.486905836551548832E-16, 1.000000000000000000 ) ) ;
#4189 = EDGE_CURVE ( 'NONE', #13452, #12639, #10914, .T. ) ;
#4190 = DIRECTION ( 'NONE',  ( 0.000000000000000000, -0.1391731009600641333, -0.9902680687415704730 ) ) ;
#4191 = ORIENTED_EDGE ( 'NONE', *, *, #11111, .F. ) ;
#4192 = CARTESIAN_POINT ( 'NONE',  ( 201.3402840685550643, 32.17245832385849980, -2.180909807981465054 ) ) ;
#4193 = CARTESIAN_POINT ( 'NONE',  ( -76.00000000000001421, -179.3058001507315282, -29.88378295107906268 ) ) ;
#4194 = PLANE ( 'NONE',  #14607 ) ;
#4195 = FACE_OUTER_BOUND ( 'NONE', #4022, .T. ) ;
#4197 = EDGE_CURVE ( 'NONE', #13871, #12666, #9815, .T. ) ;
#4196 = EDGE_CURVE ( 'NONE', #227, #6305, #2380, .T. ) ;
#4198 = EDGE_CURVE ( 'NONE', #1780, #5430, #6011, .T. ) ;
#4199 = VECTOR ( 'NONE', #7498, 1000.000000000000000 ) ;
#4200 = DIRECTION ( 'NONE',  ( 0.000000000000000000, 0.000000000000000000, -1.000000000000000000 ) ) ;
#4201 = ADVANCED_FACE ( 'NONE', ( #10835 ), #2241, .T. ) ;
#4202 = DIRECTION ( 'NONE',  ( 3.965082230804130220E-16, 0.000000000000000000, 1.000000000000000000 ) ) ;
#4203 = ORIENTED_EDGE ( 'NONE', *, *, #8449, .F. ) ;
#4204 = CARTESIAN_POINT ( 'NONE',  ( -164.5262273476079713, 106.7842295329138835, 5.000000000000000000 ) ) ;
#4205 = CARTESIAN_POINT ( 'NONE',  ( -186.0388298304660282, 135.7737150272329529, -2.963320117457103109 ) ) ;
#4206 = CARTESIAN_POINT ( 'NONE',  ( -152.4086188282879277, 107.2728346664360259, 0.000000000000000000 ) ) ;
#4207 = EDGE_LOOP ( 'NONE', ( #394, #13903, #12494, #9455 ) ) ;
#4208 = CARTESIAN_POINT ( 'NONE',  ( -173.7799404587539698, 116.1630799793301350, 5.180112981087466650 ) ) ;
#4209 = CARTESIAN_POINT ( 'NONE',  ( 190.5757627275658876, 33.76246512414177658, -1.122914728280356433 ) ) ;
#4210 = ORIENTED_EDGE ( 'NONE', *, *, #392, .F. ) ;
#4211 = EDGE_CURVE ( 'NONE', #9404, #6055, #6176, .T. ) ;
#4212 = CARTESIAN_POINT ( 'NONE',  ( -76.00000000000001421, -179.8058001507315566, -51.45141194869120937 ) ) ;
#4213 = DIRECTION ( 'NONE',  ( 0.000000000000000000, 0.000000000000000000, -1.000000000000000000 ) ) ;
#4214 = EDGE_CURVE ( 'NONE', #5867, #12589, #14596, .T. ) ;
#4215 = DIRECTION ( 'NONE',  ( -0.000000000000000000, -0.000000000000000000, 1.000000000000000000 ) ) ;
#4216 = VECTOR ( 'NONE', #15519, 1000.000000000000000 ) ;
#4217 = ADVANCED_FACE ( 'NONE', ( #4662 ), #8318, .F. ) ;
#4218 = FACE_OUTER_BOUND ( 'NONE', #10868, .T. ) ;
#4219 = ORIENTED_EDGE ( 'NONE', *, *, #14560, .T. ) ;
#4220 = DIRECTION ( 'NONE',  ( 0.000000000000000000, 0.000000000000000000, 1.000000000000000000 ) ) ;
#4221 = CARTESIAN_POINT ( 'NONE',  ( -189.6066827460468858, 129.2255495722319836, 9.577123744044220288 ) ) ;
#4222 = DIRECTION ( 'NONE',  ( -0.000000000000000000, -0.000000000000000000, 1.000000000000000000 ) ) ;
#4223 = CARTESIAN_POINT ( 'NONE',  ( 184.0000000000000568, 17.53993994372673981, -12.49999999999999467 ) ) ;
#4224 = EDGE_LOOP ( 'NONE', ( #5100, #4732, #4988, #5158, #14208 ) ) ;
#4225 = CARTESIAN_POINT ( 'NONE',  ( -76.50000000000001421, -179.3058001507315566, 52.19066787724494816 ) ) ;
#4226 = EDGE_CURVE ( 'NONE', #3135, #3829, #296, .T. ) ;
#4227 = AXIS2_PLACEMENT_3D ( 'NONE', #13710, #2914, #14660 ) ;
#4228 = ORIENTED_EDGE ( 'NONE', *, *, #10592, .F. ) ;
#4229 = ORIENTED_EDGE ( 'NONE', *, *, #229, .F. ) ;
#4230 = CARTESIAN_POINT ( 'NONE',  ( -150.9149403963819225, 108.1527335970315420, 9.827040175762299157 ) ) ;
#4231 = DIRECTION ( 'NONE',  ( 0.000000000000000000, 0.000000000000000000, 1.000000000000000000 ) ) ;
#4232 = AXIS2_PLACEMENT_3D ( 'NONE', #4459, #14168, #8038 ) ;
#4233 = SURFACE_SIDE_STYLE ('',( #1792 ) ) ;
#4234 = CARTESIAN_POINT ( 'NONE',  ( -168.6364115625881084, 126.0940691691992441, 7.458761130116111637 ) ) ;
#4235 = CARTESIAN_POINT ( 'NONE',  ( -70.00000000000000000, 15.53993994372673981, -12.49999999999999289 ) ) ;
#4236 = DIRECTION ( 'NONE',  ( 0.000000000000000000, 0.000000000000000000, 1.000000000000000000 ) ) ;
#4237 = AXIS2_PLACEMENT_3D ( 'NONE', #11236, #8875, #2948 ) ;
#4238 = CARTESIAN_POINT ( 'NONE',  ( -76.50000000000001421, 15.17911304468679923, 9.062306170389897275 ) ) ;
#4239 = PLANE ( 'NONE',  #1099 ) ;
#4240 = AXIS2_PLACEMENT_3D ( 'NONE', #13926, #8893, #15093 ) ;
#4241 = DIRECTION ( 'NONE',  ( 0.000000000000000000, 0.000000000000000000, 1.000000000000000000 ) ) ;
#4242 = CARTESIAN_POINT ( 'NONE',  ( -76.00000000000001421, 15.53993994372673804, 24.94742576086838781 ) ) ;
#4243 = VERTEX_POINT ( 'NONE', #1573 ) ;
#4244 = ADVANCED_FACE ( 'NONE', ( #13488 ), #12536, .F. ) ;
#4245 = ORIENTED_EDGE ( 'NONE', *, *, #10393, .F. ) ;
#4246 = CARTESIAN_POINT ( 'NONE',  ( 0.3173508448886631639, -8.480771745766420011, -1.310872448937987489 ) ) ;
#4247 = CARTESIAN_POINT ( 'NONE',  ( 190.0000000000000568, 15.53993994372673981, -17.50000000000002487 ) ) ;
#4248 = ORIENTED_EDGE ( 'NONE', *, *, #7157, .F. ) ;
#4249 = LINE ( 'NONE', #12625, #3392 ) ;
#4250 = CARTESIAN_POINT ( 'NONE',  ( 165.1224552381025887, 111.1124422548786299, 5.000000000000000000 ) ) ;
#4251 = CIRCLE ( 'NONE', #1990, 0.5000000000000004441 ) ;
#4252 = CIRCLE ( 'NONE', #11330, 1.699999999999993072 ) ;
#4253 = FACE_OUTER_BOUND ( 'NONE', #1938, .T. ) ;
#4254 = VERTEX_POINT ( 'NONE', #3947 ) ;
#4255 = APPLICATION_PROTOCOL_DEFINITION ( 'draft international standard', 'automotive_design', 1998, #10193 ) ;
#4256 = ORIENTED_EDGE ( 'NONE', *, *, #13041, .T. ) ;
#4257 = AXIS2_PLACEMENT_3D ( 'NONE', #2399, #3822, #1520 ) ;
#4258 = CARTESIAN_POINT ( 'NONE',  ( 207.0737247153217311, 35.51262227952910422, -0.2377773810599485560 ) ) ;
#4259 = CARTESIAN_POINT ( 'NONE',  ( -76.50000000000004263, -178.8058001507315566, 52.19066787724494816 ) ) ;
#4260 = ORIENTED_EDGE ( 'NONE', *, *, #13091, .T. ) ;
#4261 = LINE ( 'NONE', #1744, #10230 ) ;
#4262 =( GEOMETRIC_REPRESENTATION_CONTEXT ( 3 ) GLOBAL_UNCERTAINTY_ASSIGNED_CONTEXT ( ( #5792 ) ) GLOBAL_UNIT_ASSIGNED_CONTEXT ( ( #5834, #14035, #2198 ) ) REPRESENTATION_CONTEXT ( 'NONE', 'WORKASPACE' ) );
#4263 = FACE_OUTER_BOUND ( 'NONE', #130, .T. ) ;
#4264 = VERTEX_POINT ( 'NONE', #13563 ) ;
#4265 = EDGE_LOOP ( 'NONE', ( #9334, #11185 ) ) ;
#4266 = CARTESIAN_POINT ( 'NONE',  ( 175.9483885134608272, -178.8058001507315566, -30.31842631998718574 ) ) ;
#4267 = ADVANCED_FACE ( 'NONE', ( #11142 ), #4099, .F. ) ;
#4268 = DIRECTION ( 'NONE',  ( 0.000000000000000000, -1.000000000000000000, 0.000000000000000000 ) ) ;
#4269 = ORIENTED_EDGE ( 'NONE', *, *, #12897, .F. ) ;
#4270 = CARTESIAN_POINT ( 'NONE',  ( 193.1265229109121435, 35.50728864820005981, -5.680987958736793075 ) ) ;
#4271 = DIRECTION ( 'NONE',  ( -0.000000000000000000, 1.000000000000000000, -0.000000000000000000 ) ) ;
#4272 = AXIS2_PLACEMENT_3D ( 'NONE', #14169, #8277, #12828 ) ;
#4273 = CIRCLE ( 'NONE', #11592, 2.749999999999999112 ) ;
#4274 = DIRECTION ( 'NONE',  ( 1.000000000000000000, 0.000000000000000000, 0.000000000000000000 ) ) ;
#4275 = DIRECTION ( 'NONE',  ( 0.000000000000000000, 1.000000000000000000, 0.000000000000000000 ) ) ;
#4276 = LINE ( 'NONE', #4514, #6057 ) ;
#4277 = EDGE_CURVE ( 'NONE', #6520, #2617, #970, .T. ) ;
#4278 = FACE_BOUND ( 'NONE', #11004, .T. ) ;
#4279 = CIRCLE ( 'NONE', #13107, 0.5000000000000004441 ) ;
#4280 = ORIENTED_EDGE ( 'NONE', *, *, #2663, .T. ) ;
#4281 = DIRECTION ( 'NONE',  ( 1.000000000000000000, -2.751328491981765035E-32, 3.965082230804130220E-16 ) ) ;
#4282 = VECTOR ( 'NONE', #1304, 1000.000000000000000 ) ;
#4283 = EDGE_CURVE ( 'NONE', #9509, #4058, #146, .T. ) ;
#4284 = CARTESIAN_POINT ( 'NONE',  ( -195.9617019660094570, 137.8802668252396586, -4.640918829492428621 ) ) ;
#4285 = VECTOR ( 'NONE', #6532, 1000.000000000000000 ) ;
#4286 = CARTESIAN_POINT ( 'NONE',  ( 114.0000000000000568, 64.53993994372673626, 18.50000000000035527 ) ) ;
#4287 = VERTEX_POINT ( 'NONE', #4329 ) ;
#4288 = CARTESIAN_POINT ( 'NONE',  ( -198.8906912147545540, 132.4339616203728838, -4.642206099735012970 ) ) ;
#4289 = CARTESIAN_POINT ( 'NONE',  ( 192.8460887339186343, 31.43990810023382920, -3.998601258139535819 ) ) ;
#4290 = VERTEX_POINT ( 'NONE', #15286 ) ;
#4291 = EDGE_CURVE ( 'NONE', #4760, #6556, #2069, .T. ) ;
#4292 = CARTESIAN_POINT ( 'NONE',  ( 0.000000000000000000, 0.000000000000000000, 0.000000000000000000 ) ) ;
#4293 = CARTESIAN_POINT ( 'NONE',  ( 64.00000000000005684, 62.13993994372673768, 15.00000000000070166 ) ) ;
#4294 = CIRCLE ( 'NONE', #12107, 1.699999999999993072 ) ;
#4295 = CARTESIAN_POINT ( 'NONE',  ( -85.99999999999994316, 64.53993994372673626, 15.00000000000174794 ) ) ;
#4296 = AXIS2_PLACEMENT_3D ( 'NONE', #13269, #9353, #961 ) ;
#4297 = CARTESIAN_POINT ( 'NONE',  ( 114.0000000000000568, 56.53993994372675047, 13.30000000000035776 ) ) ;
#4298 = ORIENTED_EDGE ( 'NONE', *, *, #7802, .T. ) ;
#4299 = DIRECTION ( 'NONE',  ( 0.000000000000000000, 0.000000000000000000, 1.000000000000000000 ) ) ;
#4300 = EDGE_CURVE ( 'NONE', #14293, #11510, #6722, .T. ) ;
#4301 = EDGE_CURVE ( 'NONE', #13018, #3093, #9168, .T. ) ;
#4302 = EDGE_CURVE ( 'NONE', #8562, #2806, #7556, .T. ) ;
#4303 = CARTESIAN_POINT ( 'NONE',  ( -175.8847466161772957, 123.8162673009714752, 10.09358467921856573 ) ) ;
#4304 = DIRECTION ( 'NONE',  ( -1.000000000000000000, -0.000000000000000000, -0.000000000000000000 ) ) ;
#4305 = CARTESIAN_POINT ( 'NONE',  ( -155.7763779997967504, 110.7054720168813731, -4.939346198087217310 ) ) ;
#4306 = ORIENTED_EDGE ( 'NONE', *, *, #4974, .F. ) ;
#4308 = DIRECTION ( 'NONE',  ( 0.000000000000000000, 0.000000000000000000, -1.000000000000000000 ) ) ;
#4307 = CIRCLE ( 'NONE', #14390, 1.499999999999994449 ) ;
#4309 = ORIENTED_EDGE ( 'NONE', *, *, #11257, .T. ) ;
#4310 = ORIENTED_EDGE ( 'NONE', *, *, #10324, .T. ) ;
#4311 = VECTOR ( 'NONE', #7207, 1000.000000000000000 ) ;
#4312 = CARTESIAN_POINT ( 'NONE',  ( -108.0000000000000568, 59.53993994372674337, 10.00000000000000178 ) ) ;
#4313 = DIRECTION ( 'NONE',  ( 2.751328491981765035E-32, -1.000000000000000000, -1.090924371466202084E-47 ) ) ;
#4314 = DIRECTION ( 'NONE',  ( -0.000000000000000000, 1.000000000000000000, -0.000000000000000000 ) ) ;
#4315 = DIRECTION ( 'NONE',  ( 0.000000000000000000, 0.000000000000000000, -1.000000000000000000 ) ) ;
#4316 = CARTESIAN_POINT ( 'NONE',  ( -220.4428784760110034, 152.2811923084124714, -1.958540667413632974 ) ) ;
#4317 = CARTESIAN_POINT ( 'NONE',  ( 2.000000000000000000, -3.175426480542940411, 0.000000000000000000 ) ) ;
#4318 = CIRCLE ( 'NONE', #268, 0.5000000000000004441 ) ;
#4319 = EDGE_CURVE ( 'NONE', #620, #12599, #4505, .T. ) ;
#4320 = CARTESIAN_POINT ( 'NONE',  ( 178.0000000000000853, -179.3058001507315566, 52.19066787724494816 ) ) ;
#4321 = VECTOR ( 'NONE', #925, 1000.000000000000000 ) ;
#4322 = CARTESIAN_POINT ( 'NONE',  ( 6.399999999999999467, -4.618802153517037823, -7.999999999999979572 ) ) ;
#4323 = FACE_OUTER_BOUND ( 'NONE', #4153, .T. ) ;
#4324 = DIRECTION ( 'NONE',  ( 1.000000000000000000, 0.000000000000000000, -0.000000000000000000 ) ) ;
#4325 = CARTESIAN_POINT ( 'NONE',  ( -222.0498794291112290, 149.4019978443362220, -3.065875947101888599 ) ) ;
#4326 = VERTEX_POINT ( 'NONE', #7986 ) ;
#4327 =( NAMED_UNIT ( * ) SI_UNIT ( $, .STERADIAN. ) SOLID_ANGLE_UNIT ( ) );
#4328 = ORIENTED_EDGE ( 'NONE', *, *, #5066, .T. ) ;
#4329 = CARTESIAN_POINT ( 'NONE',  ( 6.399999999999999467, 0.000000000000000000, -5.400000000000019007 ) ) ;
#4330 = FACE_OUTER_BOUND ( 'NONE', #9823, .T. ) ;
#4331 = AXIS2_PLACEMENT_3D ( 'NONE', #2598, #9710, #10898 ) ;
#4332 = CARTESIAN_POINT ( 'NONE',  ( 184.0000000000000568, 19.53993994372673626, 47.49999999999997868 ) ) ;
#4333 = FACE_OUTER_BOUND ( 'NONE', #5757, .T. ) ;
#4334 = PLANE ( 'NONE',  #12762 ) ;
#4335 = AXIS2_PLACEMENT_3D ( 'NONE', #1462, #9776, #14570 ) ;
#4336 = ADVANCED_FACE ( 'NONE', ( #7834 ), #2759, .T. ) ;
#4337 = EDGE_CURVE ( 'NONE', #13018, #5068, #13323, .T. ) ;
#4338 = CARTESIAN_POINT ( 'NONE',  ( -70.00000000000000000, -181.3058001507315566, -41.45141194869120227 ) ) ;
#4339 = ORIENTED_EDGE ( 'NONE', *, *, #7881, .F. ) ;
#4340 = EDGE_CURVE ( 'NONE', #4096, #8585, #10499, .T. ) ;
#4341 = ITEM_DEFINED_TRANSFORMATION ( 'NONE', 'NONE', #1205,  #12337 ) ;
#4342 = EDGE_LOOP ( 'NONE', ( #13187, #13739, #3428, #7435, #5061, #8953 ) ) ;
#4343 = CARTESIAN_POINT ( 'NONE',  ( 188.2949840871649485, 42.33905491644829766, -4.631930676406226688 ) ) ;
#4344 = ORIENTED_EDGE ( 'NONE', *, *, #13204, .T. ) ;
#4346 = CIRCLE ( 'NONE', #12913, 1.700000000000007061 ) ;
#4345 = AXIS2_PLACEMENT_3D ( 'NONE', #7917, #13897, #6657 ) ;
#4347 = PLANE ( 'NONE',  #7726 ) ;
#4348 = FACE_OUTER_BOUND ( 'NONE', #12072, .T. ) ;
#4349 = ORIENTED_EDGE ( 'NONE', *, *, #804, .F. ) ;
#4350 = VERTEX_POINT ( 'NONE', #12932 ) ;
#4351 = DIRECTION ( 'NONE',  ( -0.000000000000000000, 0.9902680687415702510, -0.1391731009600660485 ) ) ;
#4352 = LINE ( 'NONE', #9264, #15392 ) ;
#4353 = EDGE_LOOP ( 'NONE', ( #11819, #8906, #11787, #8967 ) ) ;
#4354 = CARTESIAN_POINT ( 'NONE',  ( 191.4249991583111523, 42.11970308376083949, -6.062475933048471433 ) ) ;
#4355 = CARTESIAN_POINT ( 'NONE',  ( -35.99999999999995026, 64.53993994372673626, 13.30000000000139870 ) ) ;
#4356 = DIRECTION ( 'NONE',  ( 1.000000000000000000, 0.000000000000000000, 0.000000000000000000 ) ) ;
#4357 = CARTESIAN_POINT ( 'NONE',  ( -5.196152422706636465, 9.000000000000001776, 0.000000000000000000 ) ) ;
#4358 = DIRECTION ( 'NONE',  ( -1.000000000000000000, 0.000000000000000000, 0.000000000000000000 ) ) ;
#4359 = B_SPLINE_CURVE_WITH_KNOTS ( 'NONE', 3,
 ( #1074, #1224, #10880, #9691, #6063, #15508, #11821, #11747 ),
 .UNSPECIFIED., .F., .F.,
 ( 4, 2, 2, 4 ),
 ( 0.02285338877108902822, 0.02519297479642219548, 0.02636276780908877737, 0.02753256082175535926 ),
 .UNSPECIFIED. ) ;
#4360 = PRODUCT_DEFINITION_SHAPE ( 'NONE', 'NONE',  #15624 ) ;
#4361 = CARTESIAN_POINT ( 'NONE',  ( 14.00000000000004086, 64.53993994372673626, 15.00000000000104983 ) ) ;
#4362 = EDGE_LOOP ( 'NONE', ( #8628, #1491, #6705, #10705 ) ) ;
#4363 = EDGE_CURVE ( 'NONE', #457, #14684, #2495, .T. ) ;
#4364 = DIRECTION ( 'NONE',  ( 3.965082230804130220E-16, -4.956352788505162775E-17, 1.000000000000000000 ) ) ;
#4365 = CARTESIAN_POINT ( 'NONE',  ( -179.9223906590855222, 134.3711564447467310, 1.515441477536284554 ) ) ;
#4366 = FACE_OUTER_BOUND ( 'NONE', #6041, .T. ) ;
#4367 = ORIENTED_EDGE ( 'NONE', *, *, #11357, .F. ) ;
#4368 = CARTESIAN_POINT ( 'NONE',  ( -197.2022238459480263, 131.7665462075744358, -4.642206099735013858 ) ) ;
#4369 = CARTESIAN_POINT ( 'NONE',  ( 211.9048830940805885, 42.38452776791458376, -2.873977808594950112 ) ) ;
#4370 = CIRCLE ( 'NONE', #821, 1.699999999999993072 ) ;
#4371 = ORIENTED_EDGE ( 'NONE', *, *, #13568, .F. ) ;
#4372 = CIRCLE ( 'NONE', #13186, 1.499999999999997558 ) ;
#4373 = CARTESIAN_POINT ( 'NONE',  ( -212.9208396868292823, 149.3434102693682917, 2.431557144026069928 ) ) ;
#4374 = DIRECTION ( 'NONE',  ( 0.4873681696970831312, 0.8731965799097676229, 0.000000000000000000 ) ) ;
#4375 = DIRECTION ( 'NONE',  ( 0.000000000000000000, -1.000000000000000000, 0.000000000000000000 ) ) ;
#4376 = EDGE_CURVE ( 'NONE', #10688, #2155, #9061, .T. ) ;
#4377 = ORIENTED_EDGE ( 'NONE', *, *, #3357, .F. ) ;
#4378 = DIRECTION ( 'NONE',  ( 0.9988021735020846670, -0.04893074910025416863, -2.132255563379979538E-15 ) ) ;
#4379 = CIRCLE ( 'NONE', #1613, 1.700000000000007061 ) ;
#4380 = CARTESIAN_POINT ( 'NONE',  ( 0.000000000000000000, 0.000000000000000000, 0.000000000000000000 ) ) ;
#4381 = VERTEX_POINT ( 'NONE', #2122 ) ;
#4382 = CARTESIAN_POINT ( 'NONE',  ( 190.0000000000000568, 15.03993994372673981, -2.075184203610571210 ) ) ;
#4383 = AXIS2_PLACEMENT_3D ( 'NONE', #8857, #1577, #12467 ) ;
#4384 = CARTESIAN_POINT ( 'NONE',  ( -217.2220691230952525, 140.9637235289241062, 7.918248976830628116 ) ) ;
#4385 = FACE_OUTER_BOUND ( 'NONE', #10020, .T. ) ;
#4386 = CARTESIAN_POINT ( 'NONE',  ( 0.01688885742776555579, 7.321065037175422674, 3.319543390096038937 ) ) ;
#4387 = ORIENTED_EDGE ( 'NONE', *, *, #9139, .F. ) ;
#4388 = DIRECTION ( 'NONE',  ( 0.000000000000000000, 0.000000000000000000, 1.000000000000000000 ) ) ;
#4389 = VERTEX_POINT ( 'NONE', #5450 ) ;
#4390 = ORIENTED_EDGE ( 'NONE', *, *, #4702, .F. ) ;
#4391 = CARTESIAN_POINT ( 'NONE',  ( -166.6414209516114795, 123.5128972754229011, 2.431557144026069928 ) ) ;
#4392 = CARTESIAN_POINT ( 'NONE',  ( -64.00000000000002842, 14.90076684276667862, 37.08491613486885541 ) ) ;
#4393 = VECTOR ( 'NONE', #13658, 1000.000000000000000 ) ;
#4394 = CARTESIAN_POINT ( 'NONE',  ( -38.32399788034579302, 48.72489408690345414, 10.00000000000000178 ) ) ;
#4395 = DIRECTION ( 'NONE',  ( 0.000000000000000000, 0.000000000000000000, 1.000000000000000000 ) ) ;
#4396 = CARTESIAN_POINT ( 'NONE',  ( -221.3196620123036951, 146.4694855639384912, -4.679075448335836107 ) ) ;
#4397 = ADVANCED_FACE ( 'NONE', ( #8064, #4484 ), #928, .T. ) ;
#4399 = EDGE_CURVE ( 'NONE', #13797, #14752, #12322, .T. ) ;
#4398 = ADVANCED_FACE ( 'NONE', ( #2040 ), #6876, .T. ) ;
#4400 = DIRECTION ( 'NONE',  ( -1.000000000000000000, -0.000000000000000000, -0.000000000000000000 ) ) ;
#4401 = CARTESIAN_POINT ( 'NONE',  ( -155.6477983077465410, 110.1970436846185066, 5.000000000000004441 ) ) ;
#4402 = EDGE_CURVE ( 'NONE', #5220, #3389, #13834, .T. ) ;
#4403 = CYLINDRICAL_SURFACE ( 'NONE', #6157, 1.699999999999993072 ) ;
#4404 = FACE_OUTER_BOUND ( 'NONE', #4224, .T. ) ;
#4405 = DIRECTION ( 'NONE',  ( -1.000000000000000000, 0.000000000000000000, 0.000000000000000000 ) ) ;
#4406 = CARTESIAN_POINT ( 'NONE',  ( -219.5587625783448971, 153.8652247218668379, 0.6104961446958759863 ) ) ;
#4407 = ORIENTED_EDGE ( 'NONE', *, *, #5524, .T. ) ;
#4408 = ORIENTED_EDGE ( 'NONE', *, *, #5952, .F. ) ;
#4409 = DIRECTION ( 'NONE',  ( -1.000000000000000000, 0.000000000000000000, 0.000000000000000000 ) ) ;
#4410 = DIRECTION ( 'NONE',  ( 0.000000000000000000, 0.000000000000000000, -1.000000000000000000 ) ) ;
#4411 = ORIENTED_EDGE ( 'NONE', *, *, #9191, .F. ) ;
#4412 = PRESENTATION_STYLE_ASSIGNMENT (( #12935 ) ) ;
#4413 = CARTESIAN_POINT ( 'NONE',  ( 184.0000000000000568, 15.53993994372673981, -10.99999999999999645 ) ) ;
#4414 = CIRCLE ( 'NONE', #8474, 1.499999999999997780 ) ;
#4415 = CARTESIAN_POINT ( 'NONE',  ( 190.0000000000000568, -178.6666270497714777, -18.18093594598673945 ) ) ;
#4416 = ORIENTED_EDGE ( 'NONE', *, *, #14190, .F. ) ;
#4417 = CONTEXT_DEPENDENT_SHAPE_REPRESENTATION ( #12093, #9293 ) ;
#4418 = VERTEX_POINT ( 'NONE', #4644 ) ;
#4419 = CARTESIAN_POINT ( 'NONE',  ( 203.8319104552679448, 51.73948369304471839, -2.483607112462900446 ) ) ;
#4420 = ORIENTED_EDGE ( 'NONE', *, *, #2378, .F. ) ;
#4421 = CARTESIAN_POINT ( 'NONE',  ( 13.88529453487718968, 40.04259805664093363, 10.00000000000000178 ) ) ;
#4422 = CIRCLE ( 'NONE', #15504, 1.700000000000000178 ) ;
#4423 = CARTESIAN_POINT ( 'NONE',  ( 190.0000000000000568, 16.03993994372673981, -3.075184203610571654 ) ) ;
#4424 = ORIENTED_EDGE ( 'NONE', *, *, #13659, .F. ) ;
#4425 = EDGE_LOOP ( 'NONE', ( #13324, #13214, #10783, #11081 ) ) ;
#4426 = FACE_OUTER_BOUND ( 'NONE', #10145, .T. ) ;
#4427 = CIRCLE ( 'NONE', #15003, 1.499999999999994449 ) ;
#4428 = CARTESIAN_POINT ( 'NONE',  ( 64.00000000000005684, 62.13993994372673768, 11.50000000000069811 ) ) ;
#4429 = ADVANCED_FACE ( 'NONE', ( #7196 ), #13578, .T. ) ;
#4430 = VERTEX_POINT ( 'NONE', #14499 ) ;
#4431 = CARTESIAN_POINT ( 'NONE',  ( 178.0000000000000853, -179.8058001507315566, -51.45141194869119516 ) ) ;
#4432 = DIRECTION ( 'NONE',  ( 0.8731965799097690661, -0.4873681696970805222, 0.000000000000000000 ) ) ;
#4433 = CARTESIAN_POINT ( 'NONE',  ( 17.41029453487719181, 40.04259805664093363, 7.600000000000002309 ) ) ;
#4434 = CARTESIAN_POINT ( 'NONE',  ( 185.1062858801516882, 55.86394065090267702, 18.00000000000000355 ) ) ;
#4435 = CARTESIAN_POINT ( 'NONE',  ( -152.4086188282879277, 107.2728346664360259, 84.88378295107887084 ) ) ;
#4436 = VECTOR ( 'NONE', #10449, 1000.000000000000000 ) ;
#4437 = CONICAL_SURFACE ( 'NONE', #13255, 3.525000000000000355, 0.7853981633973787790 ) ;
#4438 = FACE_OUTER_BOUND ( 'NONE', #1319, .T. ) ;
#4439 = ORIENTED_EDGE ( 'NONE', *, *, #4687, .F. ) ;
#4440 = DIRECTION ( 'NONE',  ( -0.8731965799097684000, 0.4873681696970816879, 0.000000000000000000 ) ) ;
#4441 = CARTESIAN_POINT ( 'NONE',  ( -218.6225377568032684, 155.5426184521650441, -0.4568654681747655322 ) ) ;
#4442 = CYLINDRICAL_SURFACE ( 'NONE', #5278, 0.5000000000000004441 ) ;
#4443 = ORIENTED_EDGE ( 'NONE', *, *, #12145, .F. ) ;
#4444 = EDGE_CURVE ( 'NONE', #4326, #6739, #4251, .T. ) ;
#4445 = CARTESIAN_POINT ( 'NONE',  ( -176.4863952559862526, 117.0241230567913959, -0.6469977504890583875 ) ) ;
#4446 = CARTESIAN_POINT ( 'NONE',  ( 198.5110307061451067, 52.63772278181842523, -5.120705508804510586 ) ) ;
#4447 = VERTEX_POINT ( 'NONE', #9628 ) ;
#4448 = CIRCLE ( 'NONE', #15024, 1.500000000000001332 ) ;
#4449 = CARTESIAN_POINT ( 'NONE',  ( 19.11029453487719110, 40.04259805664093363, 5.000000000000000000 ) ) ;
#4450 = CARTESIAN_POINT ( 'NONE',  ( -76.00000000000001421, 15.03993994372673981, 10.05257423913146475 ) ) ;
#4451 = DIRECTION ( 'NONE',  ( -9.657073818396194363E-16, 0.9902680687415711391, -0.1391731009600592484 ) ) ;
#4452 = ORIENTED_EDGE ( 'NONE', *, *, #3486, .T. ) ;
#4453 =( NAMED_UNIT ( * ) SI_UNIT ( $, .STERADIAN. ) SOLID_ANGLE_UNIT ( ) );
#4454 = CARTESIAN_POINT ( 'NONE',  ( -85.99999999999994316, 62.13993994372673768, 16.70000000000174012 ) ) ;
#4455 = VECTOR ( 'NONE', #7580, 1000.000000000000000 ) ;
#4456 = ORIENTED_EDGE ( 'NONE', *, *, #14312, .T. ) ;
#4457 = FACE_OUTER_BOUND ( 'NONE', #976, .T. ) ;
#4458 = CARTESIAN_POINT ( 'NONE',  ( -208.4664676862339832, 144.5514869593766036, 9.578254705571838556 ) ) ;
#4459 = CARTESIAN_POINT ( 'NONE',  ( -85.27455057502459113, 65.19100426474074084, 5.000000000000000000 ) ) ;
#4460 = DIRECTION ( 'NONE',  ( 0.000000000000000000, 0.1391731009600626345, 0.9902680687415706950 ) ) ;
#4461 = ORIENTED_EDGE ( 'NONE', *, *, #6359, .F. ) ;
#4462 = CARTESIAN_POINT ( 'NONE',  ( 0.000000000000000000, 0.000000000000000000, 0.000000000000000000 ) ) ;
#4463 = EDGE_CURVE ( 'NONE', #5113, #6601, #12142, .T. ) ;
#4464 = ORIENTED_EDGE ( 'NONE', *, *, #4578, .T. ) ;
#4465 = VERTEX_POINT ( 'NONE', #2279 ) ;
#4466 = CARTESIAN_POINT ( 'NONE',  ( -70.00000000000000000, 17.53993994372673981, -12.49999999999999467 ) ) ;
#4467 = LINE ( 'NONE', #1940, #14058 ) ;
#4468 = FACE_OUTER_BOUND ( 'NONE', #7347, .T. ) ;
#4469 = CARTESIAN_POINT ( 'NONE',  ( -167.8263066260882397, 127.5454993279624745, 3.430700028191667084 ) ) ;
#4470 = CARTESIAN_POINT ( 'NONE',  ( -224.9839264852863323, 144.1451919755143081, -2.062628029334759638 ) ) ;
#4471 = DIRECTION ( 'NONE',  ( -0.9429519417310716634, 0.3294944882152614496, 0.04769714688914629408 ) ) ;
#4472 = LINE ( 'NONE', #3075, #67 ) ;
#4473 = CARTESIAN_POINT ( 'NONE',  ( 2.000000000000000000, 0.000000000000000000, 0.000000000000000000 ) ) ;
#4474 = ADVANCED_FACE ( 'NONE', ( #8300 ), #1321, .F. ) ;
#4475 = DIRECTION ( 'NONE',  ( 0.000000000000000000, 0.000000000000000000, 1.000000000000000000 ) ) ;
#4476 = CIRCLE ( 'NONE', #2982, 0.5000000000000004441 ) ;
#4477 = PLANE ( 'NONE',  #7844 ) ;
#4478 = DIRECTION ( 'NONE',  ( 1.000000000000000000, 0.000000000000000000, 0.000000000000000000 ) ) ;
#4479 = ORIENTED_EDGE ( 'NONE', *, *, #681, .F. ) ;
#4480 = CIRCLE ( 'NONE', #14302, 1.499999999999994449 ) ;
#4481 =( NAMED_UNIT ( * ) PLANE_ANGLE_UNIT ( ) SI_UNIT ( $, .RADIAN. ) );
#4482 = EDGE_CURVE ( 'NONE', #14401, #14171, #5497, .T. ) ;
#4483 = ORIENTED_EDGE ( 'NONE', *, *, #9364, .T. ) ;
#4484 = FACE_BOUND ( 'NONE', #9542, .T. ) ;
#4485 = LINE ( 'NONE', #4571, #15396 ) ;
#4486 = ORIENTED_EDGE ( 'NONE', *, *, #4402, .T. ) ;
#4487 = DIRECTION ( 'NONE',  ( -0.000000000000000000, 1.000000000000000000, -0.000000000000000000 ) ) ;
#4488 = DIRECTION ( 'NONE',  ( -0.8731965799097685110, 0.4873681696970816324, -0.000000000000000000 ) ) ;
#4489 = EDGE_CURVE ( 'NONE', #7872, #8949, #13030, .T. ) ;
#4490 = B_SPLINE_SURFACE_WITH_KNOTS ( 'NONE', 3, 3, ( 
 ( #3593, #3512, #4617, #21, #8349, #9445, #5806, #4541, #8428, #12979, #1136, #14241, #5885, #2170, #2332, #6999, #7163, #10704, #1063, #12035, #4693, #3436, #9515, #14395, #8500, #13208, #1208, #11735, #8270, #13046, #4859, #5963, #9677, #975, #2406, #4774, #13130, #6044, #7240, #14163, #10867, #11967, #9599, #15496 ),
 ( #14471, #14314, #10782, #3666, #2248, #898, #3361, #7082, #11888, #15568, #5729, #10542, #15337, #8200, #11810, #3831, #8574, #12112, #11463, #11174, #5165, #8650, #6123, #7466, #12261, #9913, #13519, #13368, #2720, #1439, #6279, #7846, #249, #14633, #5090, #9994, #4258, #4181, #12633, #13282, #13445, #5014, #623, #12341 ),
 ( #9020, #325, #3902, #1818, #14992, #4935, #5463, #7545, #13814, #11094, #2645, #3015, #10274, #14703, #1527, #15069, #11015, #2484, #14544, #8725, #9837, #6363, #7316, #1291, #10943, #95, #9755, #3746, #2566, #7396, #12186, #1366, #6204, #166, #1892, #3238, #8080, #5693, #7922, #12865, #2050, #3094, #9254, #13901 ),
 ( #13014, #2211, #12781, #6888, #12706, #9402, #3322, #6732, #1970, #5541, #9101, #9180, #11535, #2130, #8160, #11852, #3400, #863, #15298, #6964, #4496, #10354, #9330, #12942, #15149, #14047, #3165, #1021, #13979, #4343, #11619, #11772, #7997, #6807, #15226, #10588, #5617, #14202, #5847, #10666, #780, #15458, #10435, #4419 ),
 ( #7279, #2528, #132, #2447, #2370, #1331, #4733, #9641, #9481, #11054, #7433, #1406, #8465, #5921, #10745, #4820, #15530, #10828, #10983, #1172, #13170, #6239, #8536, #12076, #6004, #4654, #9558, #3707, #4975, #14589, #14277, #6091, #10908, #1255, #3473, #14436, #64, #13327, #3791, #14326, #14512, #8393, #8612, #8311 ),
 ( #13410, #2608, #13092, #2291, #7122, #7206, #1100, #14358, #3555, #12006, #6643, #2997, #7826, #4012, #1485, #6325, #366, #7589, #8763, #205, #7747, #5129, #442, #10107, #6404, #11367, #13795, #12616, #9958, #291, #1803, #11212, #14669, #14744, #3942, #11282, #8846, #2923, #11137, #525, #12459, #10182, #4165, #14899 ) ),
 .UNSPECIFIED., .T., .F., .F.,
 ( 4, 2, 4 ),
 ( 4, 2, 2, 2, 2, 2, 2, 2, 2, 2, 2, 2, 2, 2, 2, 2, 2, 2, 2, 2, 2, 4 ),
 ( 0.000000000000000000, 0.5000000000000000000, 1.000000000000000000 ),
 ( 0.000000000000000000, 0.01154246058414762008, 0.06319472280952896648, 0.1156547325041140800, 0.1678637871092111822, 0.2189476930995808979, 0.2714221776790743945, 0.3227197530690046334, 0.3747274728241424824, 0.4267432521036158555, 0.4780248536244998681, 0.5305055628088307662, 0.5815973485975094448, 0.6337991395759137170, 0.6855599279679012170, 0.7371634071600560167, 0.7894711232639126663, 0.8405207634104210346, 0.8929453349049019106, 0.9452650328228678900, 0.9965476795071586125, 1.000000000000000000 ),
 .UNSPECIFIED. ) ;
#4491 = AXIS2_PLACEMENT_3D ( 'NONE', #12242, #7522, #2701 ) ;
#4492 = DIRECTION ( 'NONE',  ( -0.000000000000000000, -0.000000000000000000, -1.000000000000000000 ) ) ;
#4493 = ORIENTED_EDGE ( 'NONE', *, *, #7219, .F. ) ;
#4494 = AXIS2_PLACEMENT_3D ( 'NONE', #11421, #12440, #13780 ) ;
#4495 = EDGE_LOOP ( 'NONE', ( #12349, #3821 ) ) ;
#4496 = CARTESIAN_POINT ( 'NONE',  ( 209.6506722393607731, 33.81364540586627498, -6.382933553887647271 ) ) ;
#4497 = CYLINDRICAL_SURFACE ( 'NONE', #5343, 0.5000000000000004441 ) ;
#4498 = ORIENTED_EDGE ( 'NONE', *, *, #15382, .F. ) ;
#4499 = FACE_OUTER_BOUND ( 'NONE', #12241, .T. ) ;
#4500 = ADVANCED_FACE ( 'NONE', ( #13080 ), #11837, .F. ) ;
#4501 = DIRECTION ( 'NONE',  ( 0.000000000000000000, 6.938893903907227145E-17, -1.000000000000000000 ) ) ;
#4502 = ADVANCED_FACE ( 'NONE', ( #14344 ), #8316, .T. ) ;
#4503 = DIRECTION ( 'NONE',  ( -1.000000000000000000, 0.000000000000000000, 0.000000000000000000 ) ) ;
#4504 = EDGE_LOOP ( 'NONE', ( #572, #5833, #4653, #5365 ) ) ;
#4505 = CIRCLE ( 'NONE', #7808, 0.5000000000000004441 ) ;
#4506 = ORIENTED_EDGE ( 'NONE', *, *, #10101, .T. ) ;
#4507 = CARTESIAN_POINT ( 'NONE',  ( 68.56535645333921991, 38.79159067395544014, 10.00000000000000178 ) ) ;
#4508 = CARTESIAN_POINT ( 'NONE',  ( 190.5000000000000568, 15.47035339324671099, -2.004865965629286872 ) ) ;
#4509 = AXIS2_PLACEMENT_3D ( 'NONE', #3196, #1058, #1362 ) ;
#4510 = TOROIDAL_SURFACE ( 'NONE', #2748, 1.000000000000000000, 0.5000000000000000000 ) ;
#4511 = ORIENTED_EDGE ( 'NONE', *, *, #10076, .T. ) ;
#4512 = CARTESIAN_POINT ( 'NONE',  ( 190.0000000000000568, 16.03993994372673981, -7.458121719691109004E-14 ) ) ;
#4513 = CARTESIAN_POINT ( 'NONE',  ( -81.77455057502459113, 65.19100426474074084, 10.00000000000000178 ) ) ;
#4514 = CARTESIAN_POINT ( 'NONE',  ( 176.0293059057019889, 61.25683321636181233, 10.00000000000000178 ) ) ;
#4516 = B_SPLINE_CURVE_WITH_KNOTS ( 'NONE', 3,
 ( #14243, #13048, #7085, #1686, #11177, #328, #12344, #9758, #9916, #3905, #13599, #8805, #6282, #9997, #13448, #5168, #483, #2569, #6522, #13681, #1530, #11249, #14780, #2648, #7710, #3972, #7469, #12264, #12189, #405, #5017, #2808, #1442, #13522, #9840, #7629, #14636, #12421, #2723, #8728, #4055, #1369, #2886, #1612 ),
 .UNSPECIFIED., .F., .F.,
 ( 4, 2, 2, 2, 2, 2, 2, 2, 2, 2, 2, 2, 2, 2, 2, 2, 2, 2, 2, 2, 2, 4 ),
 ( 0.0008097935439387997673, 0.002225919271470510382, 0.002933982135236355010, 0.003642044999002200072, 0.005058170726533871113, 0.006474296454065542154, 0.007890422181597214063, 0.008598485045363033971, 0.009306547909128853879, 0.01072267363666049370, 0.01213879936419213178, 0.01284686222795791352, 0.01355492509172369700, 0.01497105081925522753, 0.01638717654678675806, 0.01780330227431829032, 0.01851136513808408421, 0.01921942800184987116, 0.02063555372938145199, 0.02134361659314724241, 0.02205167945691303283, 0.02346780518444461713 ),
 .UNSPECIFIED. ) ;
#4515 = VECTOR ( 'NONE', #13505, 1000.000000000000000 ) ;
#4517 = EDGE_CURVE ( 'NONE', #14978, #10303, #4888, .T. ) ;
#4518 = DIRECTION ( 'NONE',  ( 0.000000000000000000, 0.000000000000000000, 1.000000000000000000 ) ) ;
#4519 = ORIENTED_EDGE ( 'NONE', *, *, #11732, .T. ) ;
#4520 = DIRECTION ( 'NONE',  ( 1.000000000000000000, 0.000000000000000000, 0.000000000000000000 ) ) ;
#4521 = CARTESIAN_POINT ( 'NONE',  ( -172.3582205330567945, 130.1389812296867774, 2.500000000525777644 ) ) ;
#4522 = DIRECTION ( 'NONE',  ( -0.7900120431063429871, 0.6130913241491365850, 0.000000000000000000 ) ) ;
#4523 = AXIS2_PLACEMENT_3D ( 'NONE', #13781, #6544, #11343 ) ;
#4524 = VERTEX_POINT ( 'NONE', #10731 ) ;
#4525 = CARTESIAN_POINT ( 'NONE',  ( -177.2366359034146512, 121.3924996022181375, -4.733667549831950261 ) ) ;
#4526 = CARTESIAN_POINT ( 'NONE',  ( 203.1202131991386182, 29.73909689272393564, -6.555651296533415717 ) ) ;
#4527 = CIRCLE ( 'NONE', #728, 1.700000000000001954 ) ;
#4528 = ORIENTED_EDGE ( 'NONE', *, *, #6461, .F. ) ;
#4529 = AXIS2_PLACEMENT_3D ( 'NONE', #5125, #7581, #14665 ) ;
#4530 = AXIS2_PLACEMENT_3D ( 'NONE', #2801, #9035, #10141 ) ;
#4531 = CARTESIAN_POINT ( 'NONE',  ( 0.000000000000000000, 2.381569860407204420, 1.375000000000001110 ) ) ;
#4532 = PLANE ( 'NONE',  #12003 ) ;
#4533 = APPLICATION_CONTEXT ( 'automotive_design' ) ;
#4534 = CARTESIAN_POINT ( 'NONE',  ( -64.00000000000002842, 16.03993994372673981, -17.50000000000002487 ) ) ;
#4535 = EDGE_CURVE ( 'NONE', #14360, #8201, #5912, .T. ) ;
#4536 = AXIS2_PLACEMENT_3D ( 'NONE', #6745, #710, #5553 ) ;
#4537 = ORIENTED_EDGE ( 'NONE', *, *, #5493, .T. ) ;
#4538 = VECTOR ( 'NONE', #12198, 1000.000000000000000 ) ;
#4539 = DIRECTION ( 'NONE',  ( 0.000000000000000000, 0.000000000000000000, 1.000000000000000000 ) ) ;
#4540 = DIRECTION ( 'NONE',  ( -0.000000000000000000, -0.000000000000000000, 1.000000000000000000 ) ) ;
#4541 = CARTESIAN_POINT ( 'NONE',  ( 207.1167095084715868, 46.15093117762712893, -7.185265714380067337 ) ) ;
#4542 = EDGE_LOOP ( 'NONE', ( #3723, #13412 ) ) ;
#4543 = FACE_OUTER_BOUND ( 'NONE', #2001, .T. ) ;
#4544 = CARTESIAN_POINT ( 'NONE',  ( -172.0064303153328638, 119.3480080297071595, 9.396848320176498959 ) ) ;
#4545 = CARTESIAN_POINT ( 'NONE',  ( -111.2071507613730290, 58.10263819636593041, 5.000000000000000000 ) ) ;
#4546 = LINE ( 'NONE', #3518, #736 ) ;
#4547 = CARTESIAN_POINT ( 'NONE',  ( 190.5000000000000568, -178.8058001507315566, 53.19066787724494816 ) ) ;
#4548 = EDGE_LOOP ( 'NONE', ( #5605, #12232 ) ) ;
#4549 = ORIENTED_EDGE ( 'NONE', *, *, #12126, .F. ) ;
#4550 = AXIS2_PLACEMENT_3D ( 'NONE', #10118, #13648, #2855 ) ;
#4551 = DIRECTION ( 'NONE',  ( 0.000000000000000000, -0.000000000000000000, 1.000000000000000000 ) ) ;
#4552 = CARTESIAN_POINT ( 'NONE',  ( -76.50000000000001421, 15.53993994372673981, 10.05257423913146475 ) ) ;
#4553 = VECTOR ( 'NONE', #6468, 1000.000000000000000 ) ;
#4554 = DIRECTION ( 'NONE',  ( 1.000000000000000000, 0.000000000000000000, 0.000000000000000000 ) ) ;
#4555 = CARTESIAN_POINT ( 'NONE',  ( 114.0000000000000568, 64.51493994372674479, 15.00000000000035172 ) ) ;
#4556 = EDGE_CURVE ( 'NONE', #8894, #13013, #15523, .T. ) ;
#4557 = CARTESIAN_POINT ( 'NONE',  ( -221.6351743891050603, 145.8627096086362371, -4.407674936793750220 ) ) ;
#4558 = CARTESIAN_POINT ( 'NONE',  ( -221.3451643498282806, 146.4827145868442528, 9.580214341060731442 ) ) ;
#4559 = DIRECTION ( 'NONE',  ( 0.000000000000000000, 0.000000000000000000, 1.000000000000000000 ) ) ;
#4560 = VECTOR ( 'NONE', #11119, 1000.000000000000227 ) ;
#4561 = AXIS2_PLACEMENT_3D ( 'NONE', #7855, #10444, #11391 ) ;
#4562 = CARTESIAN_POINT ( 'NONE',  ( -85.99999999999994316, 64.53993994372673626, 18.52500000000175007 ) ) ;
#4563 = CYLINDRICAL_SURFACE ( 'NONE', #5052, 0.5000000000000004441 ) ;
#4564 = CARTESIAN_POINT ( 'NONE',  ( 170.8293059057019718, 61.25683321636181233, 5.000000000000000000 ) ) ;
#4565 = CARTESIAN_POINT ( 'NONE',  ( -151.4086188282879277, 107.2728346664360259, 0.000000000000000000 ) ) ;
#4566 = ORIENTED_EDGE ( 'NONE', *, *, #15014, .F. ) ;
#4567 = EDGE_CURVE ( 'NONE', #15158, #2814, #1734, .T. ) ;
#4568 = CARTESIAN_POINT ( 'NONE',  ( 0.000000000000000000, 0.000000000000000000, 0.000000000000000000 ) ) ;
#4569 = ORIENTED_EDGE ( 'NONE', *, *, #6717, .T. ) ;
#4570 = CARTESIAN_POINT ( 'NONE',  ( -76.50000000000004263, 17.53993994372673626, 52.49999999999997868 ) ) ;
#4571 = CARTESIAN_POINT ( 'NONE',  ( 181.4384305232223369, 82.69763993231136112, 10.00000000000000178 ) ) ;
#4572 = DIRECTION ( 'NONE',  ( 0.000000000000000000, -1.000000000000000000, -1.156482317317871478E-16 ) ) ;
#4573 = CARTESIAN_POINT ( 'NONE',  ( -177.3557003870508595, 132.9282874014947140, 2.500000000000000000 ) ) ;
#4574 = CARTESIAN_POINT ( 'NONE',  ( 177.5000000000000853, 15.03993994372673804, 37.07518420361041933 ) ) ;
#4575 = VECTOR ( 'NONE', #14907, 1000.000000000000000 ) ;
#4576 = AXIS2_PLACEMENT_3D ( 'NONE', #1441, #251, #13210 ) ;
#4577 = EDGE_LOOP ( 'NONE', ( #14153, #4824, #7591, #6985 ) ) ;
#4578 = EDGE_CURVE ( 'NONE', #12077, #13002, #9545, .T. ) ;
#4579 = EDGE_LOOP ( 'NONE', ( #6858, #8658, #5081, #4990, #11443, #4173 ) ) ;
#4580 = DIRECTION ( 'NONE',  ( -5.518327896226369609E-17, -0.9902680687415712502, -0.1391731009600584990 ) ) ;
#4581 = ORIENTED_EDGE ( 'NONE', *, *, #5761, .F. ) ;
#4582 = CARTESIAN_POINT ( 'NONE',  ( 114.0000000000000568, 64.53993994372673626, 15.00000000000035172 ) ) ;
#4583 = CARTESIAN_POINT ( 'NONE',  ( -70.00000000000000000, 17.53993994372673981, -12.49999999999999467 ) ) ;
#4584 = CYLINDRICAL_SURFACE ( 'NONE', #7822, 3.500000000000004885 ) ;
#4585 = ORIENTED_EDGE ( 'NONE', *, *, #1603, .F. ) ;
#4586 = ORIENTED_EDGE ( 'NONE', *, *, #5953, .F. ) ;
#4587 = VECTOR ( 'NONE', #13076, 1000.000000000000000 ) ;
#4588 = DIRECTION ( 'NONE',  ( 0.000000000000000000, 0.000000000000000000, -1.000000000000000000 ) ) ;
#4589 = CARTESIAN_POINT ( 'NONE',  ( -34.79899788034579444, 48.72489408690345414, 5.000000000000000000 ) ) ;
#4590 = ORIENTED_EDGE ( 'NONE', *, *, #8098, .F. ) ;
#4591 = PLANE ( 'NONE',  #6322 ) ;
#4592 = CARTESIAN_POINT ( 'NONE',  ( 5.799999999999999822, 4.618802153516981868, -7.999999999999979572 ) ) ;
#4593 = ORIENTED_EDGE ( 'NONE', *, *, #14658, .F. ) ;
#4594 = CIRCLE ( 'NONE', #6116, 1.699999999999993072 ) ;
#4595 = EDGE_CURVE ( 'NONE', #4418, #1071, #3758, .T. ) ;
#4597 = ADVANCED_FACE ( 'NONE', ( #13005 ), #9284, .T. ) ;
#4596 = EDGE_CURVE ( 'NONE', #830, #7696, #8533, .T. ) ;
#4599 = STYLED_ITEM ( 'NONE', ( #12451 ), #269 ) ;
#4598 = AXIS2_PLACEMENT_3D ( 'NONE', #6254, #7681, #456 ) ;
#4600 = ORIENTED_EDGE ( 'NONE', *, *, #3469, .T. ) ;
#4601 = ORIENTED_EDGE ( 'NONE', *, *, #4674, .F. ) ;
#4602 = DIRECTION ( 'NONE',  ( 0.000000000000000000, 0.000000000000000000, 1.000000000000000000 ) ) ;
#4603 = LINE ( 'NONE', #15323, #14124 ) ;
#4604 = CARTESIAN_POINT ( 'NONE',  ( 2.000000000000000000, 1.587713240271468207, -2.750000000000000000 ) ) ;
#4605 = VERTEX_POINT ( 'NONE', #2515 ) ;
#4606 = CARTESIAN_POINT ( 'NONE',  ( -209.9898587843626956, 141.8296236499265035, -5.230826428279598872 ) ) ;
#4607 = CARTESIAN_POINT ( 'NONE',  ( 191.4177849616493461, 42.04274826850978286, -7.631480755160323426 ) ) ;
#4608 = ORIENTED_EDGE ( 'NONE', *, *, #15503, .F. ) ;
#4609 = AXIS2_PLACEMENT_3D ( 'NONE', #1470, #13709, #5267 ) ;
#4610 = CARTESIAN_POINT ( 'NONE',  ( 124.2806775638430281, 45.00321902537314145, 5.000000000000000000 ) ) ;
#4611 = CARTESIAN_POINT ( 'NONE',  ( 0.7145311798163189732, 4.618802153516981868, 8.000000000000007105 ) ) ;
#4612 = AXIS2_PLACEMENT_3D ( 'NONE', #3861, #13162, #11129 ) ;
#4613 = CARTESIAN_POINT ( 'NONE',  ( -64.00000000000002842, 15.10952649420676686, 25.44255979523916977 ) ) ;
#4614 = VERTEX_POINT ( 'NONE', #7737 ) ;
#4615 = DIRECTION ( 'NONE',  ( 1.000000000000000000, 0.000000000000000000, 0.000000000000000000 ) ) ;
#4616 = CARTESIAN_POINT ( 'NONE',  ( 0.1306530452037929224, 5.952467836904128617, -5.690023276062381008 ) ) ;
#4617 = CARTESIAN_POINT ( 'NONE',  ( 202.8882743124338504, 32.81631024066724933, -8.087096619718394663 ) ) ;
#4618 = ORIENTED_EDGE ( 'NONE', *, *, #10848, .F. ) ;
#4619 = CARTESIAN_POINT ( 'NONE',  ( -110.0000000000000426, 56.53993994372675047, 13.00000000000000178 ) ) ;
#4620 = CIRCLE ( 'NONE', #8921, 0.5000000000000004441 ) ;
#4621 = CARTESIAN_POINT ( 'NONE',  ( -186.4931015233695462, 122.8215886266871593, 7.918248976830652097 ) ) ;
#4622 = CARTESIAN_POINT ( 'NONE',  ( -219.4360840196855804, 154.0850226169901305, 3.058976617611859794 ) ) ;
#4623 = PRODUCT_DEFINITION_SHAPE ( 'NONE', 'NONE',  #14513 ) ;
#4624 = CARTESIAN_POINT ( 'NONE',  ( 201.8629198063431716, 32.54887535240757757, -8.146526315903498627 ) ) ;
#4625 = ORIENTED_EDGE ( 'NONE', *, *, #14912, .F. ) ;
#4626 = ORIENTED_EDGE ( 'NONE', *, *, #8290, .T. ) ;
#4627 = DIRECTION ( 'NONE',  ( -0.000000000000000000, 0.9902680687415711391, 0.1391731009600592484 ) ) ;
#4628 = DIRECTION ( 'NONE',  ( 0.000000000000000000, 0.000000000000000000, 1.000000000000000000 ) ) ;
#4629 = ADVANCED_FACE ( 'NONE', ( #14735 ), #5749, .T. ) ;
#4630 = FACE_BOUND ( 'NONE', #15114, .T. ) ;
#4631 = CARTESIAN_POINT ( 'NONE',  ( -83.57455057502457407, 65.19100426474074084, 10.00000000000000178 ) ) ;
#4632 = CARTESIAN_POINT ( 'NONE',  ( -223.1312025536231261, 147.4646377276753242, -2.512173040697494475 ) ) ;
#4633 = AXIS2_PLACEMENT_3D ( 'NONE', #9385, #12997, #2191 ) ;
#4634 = CARTESIAN_POINT ( 'NONE',  ( -157.0972765366304316, 120.0943610593438251, 0.000000000000000000 ) ) ;
#4635 = CIRCLE ( 'NONE', #14715, 1.499999999999997780 ) ;
#4636 = DIRECTION ( 'NONE',  ( 0.000000000000000000, 1.000000000000000000, -1.224646799147353207E-16 ) ) ;
#4637 = PLANE ( 'NONE',  #13286 ) ;
#4638 = DIRECTION ( 'NONE',  ( -0.000000000000000000, 1.000000000000000000, -0.000000000000000000 ) ) ;
#4639 = DIRECTION ( 'NONE',  ( -0.000000000000000000, 1.000000000000000000, -0.000000000000000000 ) ) ;
#4640 = DIRECTION ( 'NONE',  ( 0.000000000000000000, 0.000000000000000000, -1.000000000000000000 ) ) ;
#4641 = ORIENTED_EDGE ( 'NONE', *, *, #12964, .T. ) ;
#4642 = AXIS2_PLACEMENT_3D ( 'NONE', #45, #8370, #12055 ) ;
#4643 = VERTEX_POINT ( 'NONE', #10095 ) ;
#4644 = CARTESIAN_POINT ( 'NONE',  ( 15.71029453487719074, 40.04259805664093363, 0.000000000000000000 ) ) ;
#4646 = CARTESIAN_POINT ( 'NONE',  ( 172.5293059057019889, 61.25683321636181233, 7.600000000000002309 ) ) ;
#4645 = AXIS2_PLACEMENT_3D ( 'NONE', #144, #4985, #13420 ) ;
#4647 = LINE ( 'NONE', #8302, #4906 ) ;
#4648 = DIRECTION ( 'NONE',  ( 0.000000000000000000, -1.000000000000000000, 0.000000000000000000 ) ) ;
#4650 = ORIENTED_EDGE ( 'NONE', *, *, #10741, .T. ) ;
#4649 = EDGE_CURVE ( 'NONE', #7132, #2293, #1189, .T. ) ;
#4651 = VECTOR ( 'NONE', #900, 1000.000000000000000 ) ;
#4652 = B_SPLINE_CURVE_WITH_KNOTS ( 'NONE', 3,
 ( #13311, #9336, #2595, #866 ),
 .UNSPECIFIED., .F., .F.,
 ( 4, 4 ),
 ( 2.380742992393109920E-07, 0.001606744326298693154 ),
 .UNSPECIFIED. ) ;
#4653 = ORIENTED_EDGE ( 'NONE', *, *, #15388, .F. ) ;
#4654 = CARTESIAN_POINT ( 'NONE',  ( 201.1886137893777970, 49.58779752487713210, -5.375724496774349603 ) ) ;
#4655 = DIRECTION ( 'NONE',  ( -3.965082230804130220E-16, 0.000000000000000000, -1.000000000000000000 ) ) ;
#4656 = ORIENTED_EDGE ( 'NONE', *, *, #6397, .F. ) ;
#4657 = DIRECTION ( 'NONE',  ( 0.000000000000000000, 0.000000000000000000, -1.000000000000000000 ) ) ;
#4658 = FACE_OUTER_BOUND ( 'NONE', #8898, .T. ) ;
#4659 = DIRECTION ( 'NONE',  ( -0.3662838836490099337, 0.9305003370641709015, 0.002288952263120960697 ) ) ;
#4660 = VERTEX_POINT ( 'NONE', #13474 ) ;
#4661 = ORIENTED_EDGE ( 'NONE', *, *, #15012, .T. ) ;
#4662 = FACE_OUTER_BOUND ( 'NONE', #10271, .T. ) ;
#4663 = CARTESIAN_POINT ( 'NONE',  ( -133.4717610386620095, 107.2638826318553953, 5.000000000000000000 ) ) ;
#4664 = AXIS2_PLACEMENT_3D ( 'NONE', #977, #15498, #10628 ) ;
#4665 = EDGE_CURVE ( 'NONE', #10184, #9376, #1392, .T. ) ;
#4666 = ORIENTED_EDGE ( 'NONE', *, *, #11197, .T. ) ;
#4667 = CARTESIAN_POINT ( 'NONE',  ( -152.2854898295690873, 106.7746758752742124, 9.252772226370428399 ) ) ;
#4668 = FACE_BOUND ( 'NONE', #15521, .T. ) ;
#4669 = FACE_OUTER_BOUND ( 'NONE', #1652, .T. ) ;
#4670 = VECTOR ( 'NONE', #5871, 1000.000000000000227 ) ;
#4671 = VERTEX_POINT ( 'NONE', #12373 ) ;
#4672 = DIRECTION ( 'NONE',  ( 0.000000000000000000, 0.000000000000000000, 1.000000000000000000 ) ) ;
#4673 = VECTOR ( 'NONE', #14949, 1000.000000000000000 ) ;
#4674 = EDGE_CURVE ( 'NONE', #8395, #6805, #6393, .T. ) ;
#4675 = DIRECTION ( 'NONE',  ( 1.000000000000000000, 0.000000000000000000, 0.000000000000000000 ) ) ;
#4676 = DIRECTION ( 'NONE',  ( 0.000000000000000000, -4.956352788505162775E-17, 1.000000000000000000 ) ) ;
#4677 = FACE_OUTER_BOUND ( 'NONE', #15555, .T. ) ;
#4678 = EDGE_LOOP ( 'NONE', ( #11411, #1684 ) ) ;
#4679 = CARTESIAN_POINT ( 'NONE',  ( -170.8299300849453459, 127.1729693371208043, -2.992655347556774981 ) ) ;
#4680 = CARTESIAN_POINT ( 'NONE',  ( 211.8797403387081317, 42.53270508615055689, -3.012218501410035998 ) ) ;
#4681 = EDGE_LOOP ( 'NONE', ( #8358, #12568, #1905, #3903 ) ) ;
#4682 = EDGE_CURVE ( 'NONE', #11543, #11731, #4964, .T. ) ;
#4683 = EDGE_CURVE ( 'NONE', #6607, #9401, #11041, .T. ) ;
#4684 = VECTOR ( 'NONE', #9075, 1000.000000000000000 ) ;
#4685 = CARTESIAN_POINT ( 'NONE',  ( -63.50000000000002842, 15.53993994372673981, -17.50000000000002487 ) ) ;
#4686 = FACE_BOUND ( 'NONE', #9424, .T. ) ;
#4687 = EDGE_CURVE ( 'NONE', #1780, #11026, #7575, .T. ) ;
#4688 = DIRECTION ( 'NONE',  ( -0.000000000000000000, -0.000000000000000000, 1.000000000000000000 ) ) ;
#4689 = CIRCLE ( 'NONE', #6982, 0.5000000000000004441 ) ;
#4690 = ORIENTED_EDGE ( 'NONE', *, *, #1874, .T. ) ;
#4691 = APPLICATION_PROTOCOL_DEFINITION ( 'draft international standard', 'automotive_design', 1998, #12686 ) ;
#4692 =( LENGTH_UNIT ( ) NAMED_UNIT ( * ) SI_UNIT ( .MILLI., .METRE. ) );
#4693 = CARTESIAN_POINT ( 'NONE',  ( 207.1325720688761294, 35.61275714886660637, -4.804596322733623914 ) ) ;
#4694 = VERTEX_POINT ( 'NONE', #6230 ) ;
#4695 = CARTESIAN_POINT ( 'NONE',  ( 205.1062858801516597, 40.86394065090267702, 16.00000000000001421 ) ) ;
#4696 = CARTESIAN_POINT ( 'NONE',  ( -173.7799404587539698, 116.1630799793301350, 5.180112981087466650 ) ) ;
#4697 = DIRECTION ( 'NONE',  ( -5.518327896226369609E-17, 0.9902680687415712502, 0.1391731009600584990 ) ) ;
#4698 = DIRECTION ( 'NONE',  ( 0.000000000000000000, 0.9902680687415710281, -0.1391731009600611635 ) ) ;
#4699 = AXIS2_PLACEMENT_3D ( 'NONE', #11130, #2756, #1715 ) ;
#4700 = PLANE ( 'NONE',  #11134 ) ;
#4701 = TOROIDAL_SURFACE ( 'NONE', #13770, 1.000000000000000000, 0.5000000000000000000 ) ;
#4702 = EDGE_CURVE ( 'NONE', #10245, #3061, #8833, .T. ) ;
#4703 = ORIENTED_EDGE ( 'NONE', *, *, #14334, .T. ) ;
#4704 = ADVANCED_FACE ( 'NONE', ( #14804 ), #11276, .F. ) ;
#4705 = ORIENTED_EDGE ( 'NONE', *, *, #3919, .T. ) ;
#4706 = CARTESIAN_POINT ( 'NONE',  ( -213.9960106562366491, 134.6720553025416507, 2.431555724346858849 ) ) ;
#4707 = DIRECTION ( 'NONE',  ( 0.000000000000000000, -6.938893903907227145E-17, 1.000000000000000000 ) ) ;
#4708 = DIRECTION ( 'NONE',  ( 1.000000000000000000, 0.000000000000000000, 0.000000000000000000 ) ) ;
#4709 = CARTESIAN_POINT ( 'NONE',  ( 114.0000000000000568, 59.53993994372674337, 16.70000000000034746 ) ) ;
#4710 = CARTESIAN_POINT ( 'NONE',  ( -223.2496967378148724, 147.2523367962785414, -4.668145987003846642 ) ) ;
#4711 = ADVANCED_FACE ( 'NONE', ( #430 ), #13299, .F. ) ;
#4712 = LINE ( 'NONE', #918, #3611 ) ;
#4713 = CARTESIAN_POINT ( 'NONE',  ( -35.99999999999995026, 59.53993994372674337, 16.70000000000140261 ) ) ;
#4714 = CARTESIAN_POINT ( 'NONE',  ( 13.07968152355895874, 460.3807876674321165, 5.000000000000000000 ) ) ;
#4715 = CARTESIAN_POINT ( 'NONE',  ( 177.5000000000000853, 15.53993994372673626, 52.49999999999997868 ) ) ;
#4716 = EDGE_CURVE ( 'NONE', #50, #14309, #3729, .T. ) ;
#4717 = CARTESIAN_POINT ( 'NONE',  ( 0.000000000000000000, -2.381569860407202643, 1.375000000000004663 ) ) ;
#4718 = DIRECTION ( 'NONE',  ( 0.000000000000000000, 0.000000000000000000, 1.000000000000000000 ) ) ;
#4719 = ORIENTED_EDGE ( 'NONE', *, *, #1608, .T. ) ;
#4720 = ORIENTED_EDGE ( 'NONE', *, *, #3717, .F. ) ;
#4721 = CARTESIAN_POINT ( 'NONE',  ( 122.5806775638430253, 45.00321902537314145, 10.00000000000000178 ) ) ;
#4722 = DIRECTION ( 'NONE',  ( -1.000000000000000000, -0.000000000000000000, -0.000000000000000000 ) ) ;
#4723 = DIRECTION ( 'NONE',  ( -0.000000000000000000, 1.000000000000000000, -0.000000000000000000 ) ) ;
#4724 = CARTESIAN_POINT ( 'NONE',  ( -64.00000000000002842, -178.8058001507315566, -18.19066787724516843 ) ) ;
#4725 = DIRECTION ( 'NONE',  ( 1.000000000000000000, 0.000000000000000000, 0.000000000000000000 ) ) ;
#4726 = FACE_OUTER_BOUND ( 'NONE', #11382, .T. ) ;
#4727 = CARTESIAN_POINT ( 'NONE',  ( -76.00000000000001421, -179.8058001507315566, -30.31842631998718574 ) ) ;
#4728 = ORIENTED_EDGE ( 'NONE', *, *, #10294, .T. ) ;
#4729 = VECTOR ( 'NONE', #7516, 1000.000000000000114 ) ;
#4730 = EDGE_CURVE ( 'NONE', #9280, #10751, #4476, .T. ) ;
#4731 = VECTOR ( 'NONE', #8451, 1000.000000000000000 ) ;
#4732 = ORIENTED_EDGE ( 'NONE', *, *, #5370, .T. ) ;
#4733 = CARTESIAN_POINT ( 'NONE',  ( 208.7906731791537425, 42.14840350977979710, -9.001400940668622397 ) ) ;
#4734 = DIRECTION ( 'NONE',  ( -0.000000000000000000, -0.000000000000000000, 1.000000000000000000 ) ) ;
#4735 = EDGE_LOOP ( 'NONE', ( #12519, #5855, #3773, #13655 ) ) ;
#4736 = CARTESIAN_POINT ( 'NONE',  ( 64.00000000000005684, 64.53993994372673626, 15.00000000000070166 ) ) ;
#4737 = CARTESIAN_POINT ( 'NONE',  ( -225.5877652983326982, 143.0633199552225960, 4.273891064090742375 ) ) ;
#4738 = ORIENTED_EDGE ( 'NONE', *, *, #989, .F. ) ;
#4739 = ORIENTED_EDGE ( 'NONE', *, *, #9954, .T. ) ;
#4740 = LINE ( 'NONE', #7285, #8054 ) ;
#4741 = PLANE ( 'NONE',  #14650 ) ;
#4742 = ORIENTED_EDGE ( 'NONE', *, *, #2088, .F. ) ;
#4743 = VECTOR ( 'NONE', #5549, 1000.000000000000000 ) ;
#4744 = CARTESIAN_POINT ( 'NONE',  ( -64.00000000000002842, 15.03993994372673804, 37.07518420361041933 ) ) ;
#4745 =( GEOMETRIC_REPRESENTATION_CONTEXT ( 3 ) GLOBAL_UNCERTAINTY_ASSIGNED_CONTEXT ( ( #3582 ) ) GLOBAL_UNIT_ASSIGNED_CONTEXT ( ( #13313, #6153, #10654 ) ) REPRESENTATION_CONTEXT ( 'NONE', 'WORKASPACE' ) );
#4746 = CIRCLE ( 'NONE', #15313, 3.499999999999999556 ) ;
#4747 = PLANE ( 'NONE',  #13417 ) ;
#4748 = ORIENTED_EDGE ( 'NONE', *, *, #5403, .F. ) ;
#4749 = VERTEX_POINT ( 'NONE', #14576 ) ;
#4750 = AXIS2_PLACEMENT_3D ( 'NONE', #1903, #6973, #3248 ) ;
#4751 = DIRECTION ( 'NONE',  ( -0.000000000000000000, 1.000000000000000000, 1.486905836551548832E-16 ) ) ;
#4752 = CARTESIAN_POINT ( 'NONE',  ( -83.57455057502457407, 65.19100426474074084, 7.600000000000002309 ) ) ;
#4753 = AXIS2_PLACEMENT_3D ( 'NONE', #974, #2008, #4378 ) ;
#4754 = EDGE_CURVE ( 'NONE', #13295, #13013, #13398, .T. ) ;
#4755 = CYLINDRICAL_SURFACE ( 'NONE', #12975, 5.000000000000004441 ) ;
#4756 = AXIS2_PLACEMENT_3D ( 'NONE', #15342, #9450, #11664 ) ;
#4757 = DIRECTION ( 'NONE',  ( -0.000000000000000000, -0.000000000000000000, -1.000000000000000000 ) ) ;
#4758 = CARTESIAN_POINT ( 'NONE',  ( -85.27455057502459113, 65.19100426474074084, 7.600000000000002309 ) ) ;
#4759 = ORIENTED_EDGE ( 'NONE', *, *, #5973, .F. ) ;
#4760 = VERTEX_POINT ( 'NONE', #5197 ) ;
#4761 = CARTESIAN_POINT ( 'NONE',  ( -167.6561596704311512, 127.1594819807359329, -0.4629209656553701646 ) ) ;
#4762 = CARTESIAN_POINT ( 'NONE',  ( 188.3692075015854357, 39.10978640110493387, -4.508345083535985509 ) ) ;
#4763 = ORIENTED_EDGE ( 'NONE', *, *, #7953, .T. ) ;
#4764 = DIRECTION ( 'NONE',  ( 0.000000000000000000, 0.000000000000000000, 1.000000000000000000 ) ) ;
#4765 = CARTESIAN_POINT ( 'NONE',  ( 190.5000000000000568, 14.90076684276668040, -2.084916134869001958 ) ) ;
#4766 = AXIS2_PLACEMENT_3D ( 'NONE', #10576, #9472, #1010 ) ;
#4767 = EDGE_CURVE ( 'NONE', #7175, #14434, #13545, .T. ) ;
#4768 = LINE ( 'NONE', #13200, #3259 ) ;
#4769 = CIRCLE ( 'NONE', #9819, 1.499999999999992228 ) ;
#4770 = ORIENTED_EDGE ( 'NONE', *, *, #10039, .F. ) ;
#4771 = APPLICATION_PROTOCOL_DEFINITION ( 'draft international standard', 'automotive_design', 1998, #5878 ) ;
#4772 = EDGE_CURVE ( 'NONE', #7619, #13426, #2717, .T. ) ;
#4773 = DIRECTION ( 'NONE',  ( 1.000000000000000000, 0.000000000000000000, 0.000000000000000000 ) ) ;
#4774 = CARTESIAN_POINT ( 'NONE',  ( 205.4319281802536068, 33.87189768065903905, -1.932853472788024440 ) ) ;
#4775 = VERTEX_POINT ( 'NONE', #2834 ) ;
#4776 = CYLINDRICAL_SURFACE ( 'NONE', #14654, 1.699999999999993072 ) ;
#4777 = DIRECTION ( 'NONE',  ( -0.000000000000000000, -0.000000000000000000, 1.000000000000000000 ) ) ;
#4778 = CARTESIAN_POINT ( 'NONE',  ( -221.7331157600676192, 141.5908957077777188, 3.478895870929496148 ) ) ;
#4779 = VECTOR ( 'NONE', #14304, 1000.000000000000000 ) ;
#4780 = FACE_OUTER_BOUND ( 'NONE', #8261, .T. ) ;
#4781 = ORIENTED_EDGE ( 'NONE', *, *, #4093, .T. ) ;
#4782 = CARTESIAN_POINT ( 'NONE',  ( -179.8866491758529094, 122.3521977864031243, 9.530069280832647038 ) ) ;
#4783 = CARTESIAN_POINT ( 'NONE',  ( -167.7990583880505824, 127.5943188236592363, 2.500000001005440620 ) ) ;
#4784 = ORIENTED_EDGE ( 'NONE', *, *, #12679, .T. ) ;
#4785 = ORIENTED_EDGE ( 'NONE', *, *, #8785, .T. ) ;
#4786 = DIRECTION ( 'NONE',  ( -0.000000000000000000, -4.956352788505162775E-17, 1.000000000000000000 ) ) ;
#4787 = CARTESIAN_POINT ( 'NONE',  ( -108.0000000000000568, 59.53993994372674337, 10.00000000000000178 ) ) ;
#4788 = CARTESIAN_POINT ( 'NONE',  ( 0.000000000000000000, 0.000000000000000000, 8.000000000000007105 ) ) ;
#4789 = DIRECTION ( 'NONE',  ( 0.000000000000000000, 0.000000000000000000, 1.000000000000000000 ) ) ;
#4790 = AXIS2_PLACEMENT_3D ( 'NONE', #2183, #8282, #14174 ) ;
#4791 = DIRECTION ( 'NONE',  ( -0.000000000000000000, -1.000000000000000000, -0.000000000000000000 ) ) ;
#4792 = CIRCLE ( 'NONE', #6821, 3.525000000000000355 ) ;
#4793 = CONICAL_SURFACE ( 'NONE', #4529, 3.525000000000000355, 0.7853981633973787790 ) ;
#4794 = DIRECTION ( 'NONE',  ( -1.000000000000000000, -0.000000000000000000, -0.000000000000000000 ) ) ;
#4795 = CIRCLE ( 'NONE', #12590, 8.000000000000028422 ) ;
#4796 = EDGE_CURVE ( 'NONE', #7924, #11968, #10295, .T. ) ;
#4797 = EDGE_CURVE ( 'NONE', #14289, #11744, #8680, .T. ) ;
#4798 = CARTESIAN_POINT ( 'NONE',  ( 0.4973051450695574749, -3.866309095700866116, -7.999999999999979572 ) ) ;
#4799 = CARTESIAN_POINT ( 'NONE',  ( 68.56535645333921991, 38.79159067395544014, 0.000000000000000000 ) ) ;
#4800 = CARTESIAN_POINT ( 'NONE',  ( -156.1150904971695752, 109.3129567513242080, 9.406539233868645766 ) ) ;
#4801 = CARTESIAN_POINT ( 'NONE',  ( 162.8786896253216412, 17.13408854601560449, -5.884700754135287148 ) ) ;
#4802 = CIRCLE ( 'NONE', #14615, 7.499999999999999112 ) ;
#4803 = FACE_OUTER_BOUND ( 'NONE', #6266, .T. ) ;
#4804 = VERTEX_POINT ( 'NONE', #9300 ) ;
#4805 = CIRCLE ( 'NONE', #10363, 1.700000000000007061 ) ;
#4806 = AXIS2_PLACEMENT_3D ( 'NONE', #10313, #15105, #13693 ) ;
#4807 = ORIENTED_EDGE ( 'NONE', *, *, #4291, .F. ) ;
#4808 = CARTESIAN_POINT ( 'NONE',  ( -157.0972765366304316, 120.0943610593438251, 0.000000000000000000 ) ) ;
#4809 = CARTESIAN_POINT ( 'NONE',  ( 171.7208925888976978, 62.57671370024034729, -0.9107274384406883749 ) ) ;
#4810 = DIRECTION ( 'NONE',  ( 1.000000000000000000, 0.000000000000000000, 0.000000000000000000 ) ) ;
#4811 = CARTESIAN_POINT ( 'NONE',  ( 178.0000000000000853, -178.8058001507315566, 65.31842631998698323 ) ) ;
#4812 = LINE ( 'NONE', #1014, #10013 ) ;
#4813 = CARTESIAN_POINT ( 'NONE',  ( 177.5000000000000853, 15.10952649420676863, 9.557440204760681013 ) ) ;
#4814 = CARTESIAN_POINT ( 'NONE',  ( -201.8702151432138692, 146.6006509202294410, 3.478855109513426580 ) ) ;
#4815 = EDGE_CURVE ( 'NONE', #259, #4660, #5667, .T. ) ;
#4816 = AXIS2_PLACEMENT_3D ( 'NONE', #3568, #8405, #13182 ) ;
#4817 = ORIENTED_EDGE ( 'NONE', *, *, #12096, .F. ) ;
#4818 = CIRCLE ( 'NONE', #13384, 1.699999999999993072 ) ;
#4819 = ORIENTED_EDGE ( 'NONE', *, *, #5843, .T. ) ;
#4820 = CARTESIAN_POINT ( 'NONE',  ( 193.1767286061335653, 35.44822858574072910, -7.249992917093472933 ) ) ;
#4821 = LINE ( 'NONE', #2373, #4311 ) ;
#4822 = ORIENTED_EDGE ( 'NONE', *, *, #10307, .F. ) ;
#4823 = CARTESIAN_POINT ( 'NONE',  ( -222.9850097917987171, 147.7265650088764346, 7.563253245014972315 ) ) ;
#4824 = ORIENTED_EDGE ( 'NONE', *, *, #1115, .T. ) ;
#4825 = ORIENTED_EDGE ( 'NONE', *, *, #1378, .T. ) ;
#4826 = CARTESIAN_POINT ( 'NONE',  ( -76.50000000000001421, -178.8058001507315566, -30.31842631998718574 ) ) ;
#4827 = CARTESIAN_POINT ( 'NONE',  ( -63.50000000000002842, 16.03993994372673626, 52.49999999999997868 ) ) ;
#4828 = AXIS2_PLACEMENT_3D ( 'NONE', #1750, #14137, #9413 ) ;
#4829 = ORIENTED_EDGE ( 'NONE', *, *, #6167, .T. ) ;
#4830 = EDGE_CURVE ( 'NONE', #4850, #9446, #3222, .T. ) ;
#4831 = FACE_OUTER_BOUND ( 'NONE', #12788, .T. ) ;
#4832 = DIRECTION ( 'NONE',  ( 0.000000000000000000, 6.938893903907227145E-17, -1.000000000000000000 ) ) ;
#4833 = EDGE_CURVE ( 'NONE', #6413, #9150, #3210, .T. ) ;
#4834 = AXIS2_PLACEMENT_3D ( 'NONE', #5965, #15570, #1685 ) ;
#4835 = EDGE_CURVE ( 'NONE', #4053, #1467, #10404, .T. ) ;
#4836 = DIRECTION ( 'NONE',  ( 1.000000000000000000, 0.000000000000000000, 0.000000000000000000 ) ) ;
#4837 = AXIS2_PLACEMENT_3D ( 'NONE', #11526, #2931, #6649 ) ;
#4838 = ORIENTED_EDGE ( 'NONE', *, *, #5398, .T. ) ;
#4839 = CARTESIAN_POINT ( 'NONE',  ( -35.99999999999995026, 64.53993994372673626, 15.00000000000139977 ) ) ;
#4840 =( REPRESENTATION_RELATIONSHIP ('NONE','NONE', #3298, #3387 ) REPRESENTATION_RELATIONSHIP_WITH_TRANSFORMATION ( #5381 )SHAPE_REPRESENTATION_RELATIONSHIP( ) );
#4841 = AXIS2_PLACEMENT_3D ( 'NONE', #8467, #6965, #3401 ) ;
#4842 = ORIENTED_EDGE ( 'NONE', *, *, #505, .F. ) ;
#4843 = LINE ( 'NONE', #11791, #10724 ) ;
#4844 = FACE_OUTER_BOUND ( 'NONE', #2312, .T. ) ;
#4845 = CYLINDRICAL_SURFACE ( 'NONE', #8071, 1.499999999999994449 ) ;
#4846 = ORIENTED_EDGE ( 'NONE', *, *, #505, .T. ) ;
#4847 = ORIENTED_EDGE ( 'NONE', *, *, #11767, .T. ) ;
#4848 = CARTESIAN_POINT ( 'NONE',  ( -192.3464331062453709, 140.8629472311621100, -0.4547266291960749829 ) ) ;
#4849 = CARTESIAN_POINT ( 'NONE',  ( 192.9079700310636269, 50.30505391962363149, -5.011923969639807019 ) ) ;
#4850 = VERTEX_POINT ( 'NONE', #3297 ) ;
#4851 = EDGE_CURVE ( 'NONE', #2533, #8061, #15199, .T. ) ;
#4852 = PRESENTATION_LAYER_ASSIGNMENT (  '', '', ( #2837 ) ) ;
#4853 = FACE_OUTER_BOUND ( 'NONE', #14730, .T. ) ;
#4854 = DIRECTION ( 'NONE',  ( 0.000000000000000000, 0.000000000000000000, -1.000000000000000000 ) ) ;
#4855 = TOROIDAL_SURFACE ( 'NONE', #1314, 1.000000000000000000, 0.5000000000000000000 ) ;
#4856 = CYLINDRICAL_SURFACE ( 'NONE', #2255, 1.699999999999996625 ) ;
#4857 = EDGE_LOOP ( 'NONE', ( #2306, #11685, #11180, #10422 ) ) ;
#4858 = EDGE_CURVE ( 'NONE', #4524, #6229, #12678, .T. ) ;
#4859 = CARTESIAN_POINT ( 'NONE',  ( 191.4227524587821279, 39.61567282607229856, -2.929995994935606252 ) ) ;
#4860 = ORIENTED_EDGE ( 'NONE', *, *, #14993, .T. ) ;
#4861 = CARTESIAN_POINT ( 'NONE',  ( 73.76535645333923696, 38.79159067395544014, 9.975000000000001421 ) ) ;
#4862 = LINE ( 'NONE', #1294, #6940 ) ;
#4863 = CARTESIAN_POINT ( 'NONE',  ( -184.9748306402843809, 119.2867206268225999, 1.515400478619091995 ) ) ;
#4864 = EDGE_CURVE ( 'NONE', #13446, #6990, #8774, .T. ) ;
#4865 = DIRECTION ( 'NONE',  ( 1.000000000000000000, 0.000000000000000000, 0.000000000000000000 ) ) ;
#4866 = EDGE_LOOP ( 'NONE', ( #9285, #3976, #9808 ) ) ;
#4867 = CARTESIAN_POINT ( 'NONE',  ( -204.1871669930114024, 142.4247710585700020, 9.578254705571842109 ) ) ;
#4868 = VECTOR ( 'NONE', #9732, 1000.000000000000000 ) ;
#4869 = CARTESIAN_POINT ( 'NONE',  ( -63.50000000000002842, -178.9449732516916072, -29.32815825124560760 ) ) ;
#4870 = ORIENTED_EDGE ( 'NONE', *, *, #13262, .T. ) ;
#4871 = ORIENTED_EDGE ( 'NONE', *, *, #5707, .F. ) ;
#4872 = CARTESIAN_POINT ( 'NONE',  ( -191.4963330474078020, 125.7496346496455004, 2.431555724346856184 ) ) ;
#4873 = DIRECTION ( 'NONE',  ( -1.000000000000000000, 0.000000000000000000, 0.000000000000000000 ) ) ;
#4874 = EDGE_CURVE ( 'NONE', #14286, #5616, #4467, .T. ) ;
#4875 = CARTESIAN_POINT ( 'NONE',  ( 70.26535645333922275, 38.79159067395544014, 7.600000000000002309 ) ) ;
#4876 = DIRECTION ( 'NONE',  ( 0.000000000000000000, -0.000000000000000000, 1.000000000000000000 ) ) ;
#4877 = DIRECTION ( 'NONE',  ( -0.000000000000000000, 1.000000000000000000, 6.938893903907227145E-17 ) ) ;
#4878 = CARTESIAN_POINT ( 'NONE',  ( -217.4370776556141607, 153.6126725021986772, 6.955470517783211903 ) ) ;
#4879 = CIRCLE ( 'NONE', #15446, 1.499999999999994449 ) ;
#4880 = CARTESIAN_POINT ( 'NONE',  ( 14.00000000000004086, 64.53993994372673626, 15.00000000000104983 ) ) ;
#4881 = FACE_OUTER_BOUND ( 'NONE', #5835, .T. ) ;
#4882 = AXIS2_PLACEMENT_3D ( 'NONE', #13952, #8050, #4554 ) ;
#4883 = CARTESIAN_POINT ( 'NONE',  ( -211.2987210398670186, 151.8733316563206586, 2.500000000000000000 ) ) ;
#4884 = DIRECTION ( 'NONE',  ( -0.000000000000000000, -0.000000000000000000, 1.000000000000000000 ) ) ;
#4885 = DIRECTION ( 'NONE',  ( -1.000000000000000000, -0.000000000000000000, -0.000000000000000000 ) ) ;
#4886 = ORIENTED_EDGE ( 'NONE', *, *, #948, .F. ) ;
#4887 = ORIENTED_EDGE ( 'NONE', *, *, #13436, .T. ) ;
#4888 = LINE ( 'NONE', #2436, #6542 ) ;
#4889 = FACE_OUTER_BOUND ( 'NONE', #6374, .T. ) ;
#4890 = CARTESIAN_POINT ( 'NONE',  ( 177.5000000000000853, -179.8058001507315566, -51.45141194869120227 ) ) ;
#4891 = EDGE_CURVE ( 'NONE', #411, #868, #3137, .T. ) ;
#4892 = CYLINDRICAL_SURFACE ( 'NONE', #10676, 0.5000000000000004441 ) ;
#4893 = DIRECTION ( 'NONE',  ( -0.000000000000000000, 0.000000000000000000, 1.000000000000000000 ) ) ;
#4895 = ADVANCED_FACE ( 'NONE', ( #11672 ), #833, .T. ) ;
#4894 = EDGE_CURVE ( 'NONE', #6169, #2150, #752, .T. ) ;
#4896 = DIRECTION ( 'NONE',  ( -1.000000000000000000, -0.000000000000000000, -0.000000000000000000 ) ) ;
#4897 = CARTESIAN_POINT ( 'NONE',  ( -211.3030747601025610, 151.8655312830997559, 3.478855109513426580 ) ) ;
#4898 = AXIS2_PLACEMENT_3D ( 'NONE', #9530, #14645, #3763 ) ;
#4899 = EDGE_CURVE ( 'NONE', #5616, #5655, #13951, .T. ) ;
#4900 = ORIENTED_EDGE ( 'NONE', *, *, #5741, .F. ) ;
#4901 = AXIS2_PLACEMENT_3D ( 'NONE', #11746, #6777, #10403 ) ;
#4902 = EDGE_LOOP ( 'NONE', ( #6966, #12151, #8726, #1661 ) ) ;
#4903 = AXIS2_PLACEMENT_3D ( 'NONE', #7979, #843, #9310 ) ;
#4904 = CARTESIAN_POINT ( 'NONE',  ( -70.00000000000000000, 19.53993994372674337, -12.49999999999999467 ) ) ;
#4905 = ORIENTED_EDGE ( 'NONE', *, *, #7414, .T. ) ;
#4906 = VECTOR ( 'NONE', #13083, 1000.000000000000000 ) ;
#4907 = CARTESIAN_POINT ( 'NONE',  ( -222.0618215705420369, 145.1005326155232922, 8.841470136485687803 ) ) ;
#4908 = ORIENTED_EDGE ( 'NONE', *, *, #13060, .T. ) ;
#4909 = LINE ( 'NONE', #9647, #6799 ) ;
#4910 = CARTESIAN_POINT ( 'NONE',  ( 201.7654193689693045, 29.10045082804961325, -2.190250528083291570 ) ) ;
#4911 = EDGE_CURVE ( 'NONE', #11614, #2480, #426, .T. ) ;
#4912 = VERTEX_POINT ( 'NONE', #14097 ) ;
#4913 = CARTESIAN_POINT ( 'NONE',  ( 177.5000000000000568, 19.53993994372674337, 24.99999999999999645 ) ) ;
#4914 = LINE ( 'NONE', #7369, #14121 ) ;
#4915 = TOROIDAL_SURFACE ( 'NONE', #9968, 6.999999999999991118, 2.000000000000000000 ) ;
#4916 = FACE_OUTER_BOUND ( 'NONE', #1053, .T. ) ;
#4917 = EDGE_CURVE ( 'NONE', #4749, #9433, #8133, .T. ) ;
#4918 = VERTEX_POINT ( 'NONE', #11513 ) ;
#4919 =( LENGTH_UNIT ( ) NAMED_UNIT ( * ) SI_UNIT ( .MILLI., .METRE. ) );
#4920 = EDGE_LOOP ( 'NONE', ( #15154, #8510, #11524, #2524 ) ) ;
#4921 = FACE_BOUND ( 'NONE', #1672, .T. ) ;
#4922 = EDGE_CURVE ( 'NONE', #2806, #8562, #11803, .T. ) ;
#4923 = VECTOR ( 'NONE', #15169, 1000.000000000000000 ) ;
#4924 = CARTESIAN_POINT ( 'NONE',  ( -168.8345777152483151, 119.5835126658289909, 2.431557144026069928 ) ) ;
#4925 = EDGE_LOOP ( 'NONE', ( #9126, #15617, #14053, #6671 ) ) ;
#4926 = VERTEX_POINT ( 'NONE', #511 ) ;
#4927 = CARTESIAN_POINT ( 'NONE',  ( -188.0666105031049824, 138.5497687542270739, -0.4547266291960739282 ) ) ;
#4928 = CARTESIAN_POINT ( 'NONE',  ( 207.2255354594468884, 50.38222520613008015, -5.636003230111601425 ) ) ;
#4929 = ORIENTED_EDGE ( 'NONE', *, *, #1719, .T. ) ;
#4930 = FACE_BOUND ( 'NONE', #15283, .T. ) ;
#4931 = DIRECTION ( 'NONE',  ( -1.000000000000000000, 0.000000000000000000, 0.000000000000000000 ) ) ;
#4932 = AXIS2_PLACEMENT_3D ( 'NONE', #10127, #5621, #2943 ) ;
#4933 = VERTEX_POINT ( 'NONE', #14963 ) ;
#4934 = CARTESIAN_POINT ( 'NONE',  ( 114.0000000000000568, 64.53993994372673626, 16.70000000000034746 ) ) ;
#4935 = CARTESIAN_POINT ( 'NONE',  ( 211.8917419932436985, 39.20340779279173660, -5.995121456379560954 ) ) ;
#4936 = ORIENTED_EDGE ( 'NONE', *, *, #2938, .F. ) ;
#4937 = DIRECTION ( 'NONE',  ( 0.000000000000000000, 0.000000000000000000, 1.000000000000000000 ) ) ;
#4938 = DIRECTION ( 'NONE',  ( 3.965082230804130220E-16, 0.000000000000000000, 1.000000000000000000 ) ) ;
#4939 = CARTESIAN_POINT ( 'NONE',  ( -181.0860728093183809, 120.2032420692993071, -3.023257939496618807 ) ) ;
#4940 = EDGE_CURVE ( 'NONE', #5473, #15212, #2464, .T. ) ;
#4941 = DIRECTION ( 'NONE',  ( 0.000000000000000000, 0.9569673715906177325, 0.2901955370279575286 ) ) ;
#4942 = EDGE_LOOP ( 'NONE', ( #546, #6060, #12457, #7673, #5946, #4390, #1148, #8475 ) ) ;
#4943 = CARTESIAN_POINT ( 'NONE',  ( -197.2254974982137128, 131.7248478061943615, 9.577123744044225617 ) ) ;
#4944 = CARTESIAN_POINT ( 'NONE',  ( 201.3139613293953971, 49.56665511821758230, -6.809528532989353344 ) ) ;
#4945 = AXIS2_PLACEMENT_3D ( 'NONE', #2294, #12945, #4657 ) ;
#4946 = ORIENTED_EDGE ( 'NONE', *, *, #10976, .F. ) ;
#4947 = VERTEX_POINT ( 'NONE', #595 ) ;
#4948 = CARTESIAN_POINT ( 'NONE',  ( 202.6027916890166694, 29.64969172180087398, -8.171549047034778468 ) ) ;
#4949 = CARTESIAN_POINT ( 'NONE',  ( 215.4200305399390345, 33.33196348269225240, 5.000000000000000000 ) ) ;
#4950 = VECTOR ( 'NONE', #12182, 999.9999999999998863 ) ;
#4951 = CARTESIAN_POINT ( 'NONE',  ( -61.94838851346079167, 15.03993994372673804, 24.94742576086838781 ) ) ;
#4952 = DIRECTION ( 'NONE',  ( -0.4873681696970814659, -0.8731965799097686221, 0.000000000000000000 ) ) ;
#4953 = DIRECTION ( 'NONE',  ( 0.000000000000000000, 8.673617379884035472E-17, -1.000000000000000000 ) ) ;
#4954 = LINE ( 'NONE', #9772, #7670 ) ;
#4955 = CIRCLE ( 'NONE', #11011, 1.699999999999993072 ) ;
#4956 = CYLINDRICAL_SURFACE ( 'NONE', #3138, 0.5000000000000004441 ) ;
#4957 = VECTOR ( 'NONE', #3375, 1000.000000000000000 ) ;
#4958 = ADVANCED_FACE ( 'NONE', ( #7969, #5433 ), #10248, .T. ) ;
#4959 = CARTESIAN_POINT ( 'NONE',  ( -179.9267697467775520, 134.3633106217456543, 2.500000000000000000 ) ) ;
#4960 = CARTESIAN_POINT ( 'NONE',  ( 114.0000000000000568, 64.53993994372673626, 18.52500000000035385 ) ) ;
#4961 = CARTESIAN_POINT ( 'NONE',  ( -130.0135953313997561, 106.9229804370480537, 5.000000000000000000 ) ) ;
#4962 = ORIENTED_EDGE ( 'NONE', *, *, #537, .T. ) ;
#4963 = ORIENTED_EDGE ( 'NONE', *, *, #7499, .T. ) ;
#4964 = LINE ( 'NONE', #7655, #1949 ) ;
#4965 = CARTESIAN_POINT ( 'NONE',  ( 0.000000000000000000, 1.836970198721029688E-16, -1.499999999999999778 ) ) ;
#4966 = CARTESIAN_POINT ( 'NONE',  ( 0.000000000000000000, 0.000000000000000000, 0.000000000000000000 ) ) ;
#4967 = FACE_BOUND ( 'NONE', #14678, .T. ) ;
#4968 = AXIS2_PLACEMENT_3D ( 'NONE', #7352, #12147, #5916 ) ;
#4969 = DIRECTION ( 'NONE',  ( -0.000000000000000000, -0.000000000000000000, 1.000000000000000000 ) ) ;
#4970 = CARTESIAN_POINT ( 'NONE',  ( -185.2098801967860595, 137.3018090142982146, 3.478855109513427468 ) ) ;
#4972 = VERTEX_POINT ( 'NONE', #3253 ) ;
#4971 = EDGE_CURVE ( 'NONE', #101, #6346, #13042, .T. ) ;
#4973 = ORIENTED_EDGE ( 'NONE', *, *, #5483, .T. ) ;
#4974 = EDGE_CURVE ( 'NONE', #14204, #908, #1452, .T. ) ;
#4975 = CARTESIAN_POINT ( 'NONE',  ( 193.0816233526163046, 46.15577860858359571, -4.879990690958216248 ) ) ;
#4976 = PRODUCT_DEFINITION ( 'UNKNOWN', '', #12817, #2843 ) ;
#4977 = CARTESIAN_POINT ( 'NONE',  ( -61.94838851346079167, 15.03993994372673981, -2.575184203610571654 ) ) ;
#4978 = EDGE_LOOP ( 'NONE', ( #1147, #2629 ) ) ;
#4979 = CARTESIAN_POINT ( 'NONE',  ( -222.4011748855326687, 148.7725968900727764, 7.888572101362996136 ) ) ;
#4980 = ORIENTED_EDGE ( 'NONE', *, *, #9956, .T. ) ;
#4981 = ADVANCED_FACE ( 'NONE', ( #15311 ), #15471, .T. ) ;
#4982 = CARTESIAN_POINT ( 'NONE',  ( -157.6477983077465694, 110.1970436846185066, 84.88378295107887084 ) ) ;
#4983 = CARTESIAN_POINT ( 'NONE',  ( 190.6253575848006960, 33.70309657413156401, -2.691919612340673673 ) ) ;
#4984 = VERTEX_POINT ( 'NONE', #10757 ) ;
#4985 = DIRECTION ( 'NONE',  ( 0.000000000000000000, -1.000000000000000000, -4.956352788505162775E-17 ) ) ;
#4986 = CARTESIAN_POINT ( 'NONE',  ( 190.0000000000000853, 23.05038067821379499, 35.93956260393299829 ) ) ;
#4987 = CARTESIAN_POINT ( 'NONE',  ( 177.5000000000000853, 15.53993994372673981, -17.50000000000002487 ) ) ;
#4988 = ORIENTED_EDGE ( 'NONE', *, *, #7139, .F. ) ;
#4989 = CIRCLE ( 'NONE', #12290, 0.5000000000000001110 ) ;
#4990 = ORIENTED_EDGE ( 'NONE', *, *, #9412, .T. ) ;
#4991 = ADVANCED_FACE ( 'NONE', ( #10678 ), #2064, .T. ) ;
#4992 = EDGE_CURVE ( 'NONE', #1333, #14712, #7083, .T. ) ;
#4993 = DIRECTION ( 'NONE',  ( 1.000000000000000000, 0.000000000000000000, 0.000000000000000000 ) ) ;
#4994 = EDGE_CURVE ( 'NONE', #10303, #9977, #13493, .T. ) ;
#4995 = VERTEX_POINT ( 'NONE', #12313 ) ;
#4996 = DIRECTION ( 'NONE',  ( -0.4999999999999997224, -0.8660254037844388186, 0.000000000000000000 ) ) ;
#4997 = VECTOR ( 'NONE', #11127, 1000.000000000000000 ) ;
#4998 = CARTESIAN_POINT ( 'NONE',  ( 190.2479883433758800, 63.36949047362622167, 5.000000000000000000 ) ) ;
#4999 = ORIENTED_EDGE ( 'NONE', *, *, #6638, .F. ) ;
#5000 = ORIENTED_EDGE ( 'NONE', *, *, #6731, .F. ) ;
#5001 = CARTESIAN_POINT ( 'NONE',  ( -177.3513212993587729, 132.9361332244957055, 1.515441477536284109 ) ) ;
#5002 = CARTESIAN_POINT ( 'NONE',  ( -223.6090965991043902, 142.0216235376909424, 2.002380365345714619 ) ) ;
#5003 = CIRCLE ( 'NONE', #10300, 3.525000000000000355 ) ;
#5004 = ORIENTED_EDGE ( 'NONE', *, *, #15572, .F. ) ;
#5005 = DIRECTION ( 'NONE',  ( 0.000000000000000000, 0.000000000000000000, 1.000000000000000000 ) ) ;
#5006 = DIRECTION ( 'NONE',  ( 1.000000000000000000, -0.000000000000000000, -0.000000000000000000 ) ) ;
#5007 = DIRECTION ( 'NONE',  ( 0.000000000000000000, 0.000000000000000000, 1.000000000000000000 ) ) ;
#5008 = EDGE_CURVE ( 'NONE', #9250, #14837, #7368, .T. ) ;
#5009 = AXIS2_PLACEMENT_3D ( 'NONE', #13508, #2872, #14845 ) ;
#5010 = EDGE_LOOP ( 'NONE', ( #11215, #5717 ) ) ;
#5011 = PRODUCT_DEFINITION_FORMATION_WITH_SPECIFIED_SOURCE ( 'ANY', '', #690, .NOT_KNOWN. ) ;
#5012 = VECTOR ( 'NONE', #648, 1000.000000000000000 ) ;
#5013 = CARTESIAN_POINT ( 'NONE',  ( -64.00000000000002842, 15.53993994372673981, 9.617930870223348805 ) ) ;
#5014 = CARTESIAN_POINT ( 'NONE',  ( 203.2853005557455788, 48.75346994511389198, 0.6442813861133344089 ) ) ;
#5015 = ORIENTED_EDGE ( 'NONE', *, *, #14306, .T. ) ;
#5016 = CARTESIAN_POINT ( 'NONE',  ( 215.1062858801516882, 55.86394065090267702, 18.00000000000000355 ) ) ;
#5017 = CARTESIAN_POINT ( 'NONE',  ( -217.8165228275882157, 152.9407092898246958, -2.993413372942824502 ) ) ;
#5018 = CARTESIAN_POINT ( 'NONE',  ( -178.4115273750087738, 119.2860570028907858, -3.078262048313290311 ) ) ;
#5019 = DIRECTION ( 'NONE',  ( -1.000000000000000000, 0.000000000000000000, 0.000000000000000000 ) ) ;
#5020 = VERTEX_POINT ( 'NONE', #11064 ) ;
#5021 = CARTESIAN_POINT ( 'NONE',  ( -194.3889542450793613, 137.0335258394182745, 9.578254705571838556 ) ) ;
#5022 = CARTESIAN_POINT ( 'NONE',  ( 203.0658429208174880, 48.83360436048501896, -0.9158339742359169477 ) ) ;
#5023 = ORIENTED_EDGE ( 'NONE', *, *, #15012, .F. ) ;
#5024 = ORIENTED_EDGE ( 'NONE', *, *, #14870, .F. ) ;
#5025 = AXIS2_PLACEMENT_3D ( 'NONE', #14116, #11761, #5756 ) ;
#5026 = VECTOR ( 'NONE', #7066, 1000.000000000000000 ) ;
#5027 = DIRECTION ( 'NONE',  ( -0.000000000000000000, -4.956352788505162775E-17, 1.000000000000000000 ) ) ;
#5028 = DIRECTION ( 'NONE',  ( 1.000000000000000000, 0.000000000000000000, 0.000000000000000000 ) ) ;
#5029 = ADVANCED_FACE ( 'NONE', ( #10840 ), #8772, .F. ) ;
#5030 = DIRECTION ( 'NONE',  ( -1.000000000000000000, 0.000000000000000000, 0.000000000000000000 ) ) ;
#5031 = VECTOR ( 'NONE', #14387, 1000.000000000000000 ) ;
#5032 = CARTESIAN_POINT ( 'NONE',  ( 0.000000000000000000, 0.000000000000000000, 0.000000000000000000 ) ) ;
#5033 = DIRECTION ( 'NONE',  ( 0.000000000000000000, 0.000000000000000000, 1.000000000000000000 ) ) ;
#5034 = CARTESIAN_POINT ( 'NONE',  ( -211.4864660300886499, 151.5260579444296525, 5.434754235172608361 ) ) ;
#5035 = DIRECTION ( 'NONE',  ( -1.000000000000000000, 0.000000000000000000, 0.000000000000000000 ) ) ;
#5036 = DIRECTION ( 'NONE',  ( -0.000000000000000000, -0.000000000000000000, -1.000000000000000000 ) ) ;
#5037 = VERTEX_POINT ( 'NONE', #4913 ) ;
#5038 = EDGE_CURVE ( 'NONE', #3389, #13605, #1263, .T. ) ;
#5039 = ORIENTED_EDGE ( 'NONE', *, *, #3750, .F. ) ;
#5040 = DIRECTION ( 'NONE',  ( -1.000000000000000000, 0.000000000000000000, 0.000000000000000000 ) ) ;
#5041 = DIRECTION ( 'NONE',  ( -0.000000000000000000, 1.000000000000000000, 6.938893903907227145E-17 ) ) ;
#5042 = SURFACE_SIDE_STYLE ('',( #6312 ) ) ;
#5043 = CIRCLE ( 'NONE', #2267, 1.499999999999994449 ) ;
#5044 = CARTESIAN_POINT ( 'NONE',  ( 0.000000000000000000, 2.381569860407203532, -1.375000000000002665 ) ) ;
#5045 = CARTESIAN_POINT ( 'NONE',  ( -76.00000000000004263, 15.53993994372673804, 38.07518420361041933 ) ) ;
#5046 = CARTESIAN_POINT ( 'NONE',  ( -85.99999999999994316, 59.53993994372674337, 15.00000000000174794 ) ) ;
#5047 = CARTESIAN_POINT ( 'NONE',  ( -174.7846310273254176, 131.4932641812416421, 2.500000000270498735 ) ) ;
#5048 = VERTEX_POINT ( 'NONE', #13569 ) ;
#5049 = PLANE ( 'NONE',  #6144 ) ;
#5050 = AXIS2_PLACEMENT_3D ( 'NONE', #6978, #10446, #875 ) ;
#5051 = EDGE_CURVE ( 'NONE', #14374, #435, #5140, .T. ) ;
#5052 = AXIS2_PLACEMENT_3D ( 'NONE', #923, #5750, #8223 ) ;
#5053 = AXIS2_PLACEMENT_3D ( 'NONE', #5417, #9055, #13854 ) ;
#5054 = CARTESIAN_POINT ( 'NONE',  ( 0.1097966057364734849, 1.070857859039281657, -2.750000000000000444 ) ) ;
#5055 = CARTESIAN_POINT ( 'NONE',  ( -224.4579709560119909, 145.0875238672886951, 4.289685626893874115 ) ) ;
#5056 = EDGE_LOOP ( 'NONE', ( #5767, #10997, #7932, #12354 ) ) ;
#5057 = CARTESIAN_POINT ( 'NONE',  ( -221.7730551926511566, 145.6605518061857083, 9.210365250596908027 ) ) ;
#5058 = ORIENTED_EDGE ( 'NONE', *, *, #9272, .T. ) ;
#5059 = CARTESIAN_POINT ( 'NONE',  ( -173.2963660003902362, 117.7450293044227294, -3.133322902959446932 ) ) ;
#5060 = CARTESIAN_POINT ( 'NONE',  ( 192.8746960878046650, 31.41537247659151433, -2.569271051570655384 ) ) ;
#5061 = ORIENTED_EDGE ( 'NONE', *, *, #9834, .T. ) ;
#5062 = DIRECTION ( 'NONE',  ( -1.000000000000000000, 0.000000000000000000, 0.000000000000000000 ) ) ;
#5063 = LINE ( 'NONE', #12540, #11118 ) ;
#5064 = AXIS2_PLACEMENT_3D ( 'NONE', #1419, #4832, #6252 ) ;
#5065 = AXIS2_PLACEMENT_3D ( 'NONE', #350, #14657, #2908 ) ;
#5066 = EDGE_CURVE ( 'NONE', #12693, #6470, #8701, .T. ) ;
#5067 = DIRECTION ( 'NONE',  ( 1.000000000000000000, 0.000000000000000000, 0.000000000000000000 ) ) ;
#5068 = VERTEX_POINT ( 'NONE', #2697 ) ;
#5069 = DIRECTION ( 'NONE',  ( 0.000000000000000000, -1.000000000000000000, 0.000000000000000000 ) ) ;
#5070 = ORIENTED_EDGE ( 'NONE', *, *, #14922, .T. ) ;
#5071 = LINE ( 'NONE', #81, #11098 ) ;
#5072 = FACE_OUTER_BOUND ( 'NONE', #9314, .T. ) ;
#5073 = ORIENTED_EDGE ( 'NONE', *, *, #6450, .F. ) ;
#5074 = CARTESIAN_POINT ( 'NONE',  ( 6.800000000000000711, 0.000000000000000000, 0.000000000000000000 ) ) ;
#5075 = CARTESIAN_POINT ( 'NONE',  ( -152.2908072257909282, 107.7606257468605833, -4.720820933574416678 ) ) ;
#5076 = ORIENTED_EDGE ( 'NONE', *, *, #1897, .T. ) ;
#5077 = VERTEX_POINT ( 'NONE', #7290 ) ;
#5078 = AXIS2_PLACEMENT_3D ( 'NONE', #15459, #4655, #5850 ) ;
#5079 = DIRECTION ( 'NONE',  ( -0.000000000000000000, 1.000000000000000000, -0.000000000000000000 ) ) ;
#5080 = CARTESIAN_POINT ( 'NONE',  ( 205.4339596421060889, 33.86846485884471747, -4.932823326473320336 ) ) ;
#5081 = ORIENTED_EDGE ( 'NONE', *, *, #5603, .T. ) ;
#5082 = DIRECTION ( 'NONE',  ( -0.000000000000000000, -0.000000000000000000, -1.000000000000000000 ) ) ;
#5083 = ADVANCED_FACE ( 'NONE', ( #3950 ), #14446, .T. ) ;
#5085 = ADVANCED_FACE ( 'NONE', ( #9802 ), #14600, .F. ) ;
#5084 = EDGE_CURVE ( 'NONE', #14585, #3344, #5657, .T. ) ;
#5086 = CARTESIAN_POINT ( 'NONE',  ( 164.0000000000000568, 64.53993994372673626, 13.29999999999999538 ) ) ;
#5087 = AXIS2_PLACEMENT_3D ( 'NONE', #1730, #1808, #7754 ) ;
#5088 = CIRCLE ( 'NONE', #7119, 1.700000000000000178 ) ;
#5089 = DIRECTION ( 'NONE',  ( 0.000000000000000000, 0.9902680687415711391, 0.1391731009600593039 ) ) ;
#5090 = CARTESIAN_POINT ( 'NONE',  ( 201.2644297667355886, 32.15691159195442594, -0.6119088838163699862 ) ) ;
#5091 = ORIENTED_EDGE ( 'NONE', *, *, #5142, .T. ) ;
#5092 = CARTESIAN_POINT ( 'NONE',  ( -76.00000000000004263, 14.90076684276667862, 37.08491613486884830 ) ) ;
#5093 = CARTESIAN_POINT ( 'NONE',  ( 164.0000000000000568, 64.53993994372673626, 15.00000000000000355 ) ) ;
#5094 = CARTESIAN_POINT ( 'NONE',  ( -189.5834090937817109, 129.2672479736120010, -4.642206099735012970 ) ) ;
#5095 = DIRECTION ( 'NONE',  ( -0.000000000000000000, 0.000000000000000000, 1.000000000000000000 ) ) ;
#5096 = ORIENTED_EDGE ( 'NONE', *, *, #6908, .F. ) ;
#5097 = CARTESIAN_POINT ( 'NONE',  ( -220.6842914767384229, 151.8486630221608209, 9.556866313350491637 ) ) ;
#5099 = CARTESIAN_POINT ( 'NONE',  ( 201.7905037730716913, 32.52922036567187547, -6.577523224799477930 ) ) ;
#5098 = CIRCLE ( 'NONE', #2577, 1.000000000000000888 ) ;
#5100 = ORIENTED_EDGE ( 'NONE', *, *, #11840, .F. ) ;
#5101 = VERTEX_POINT ( 'NONE', #6180 ) ;
#5102 = CIRCLE ( 'NONE', #3845, 0.5000000000000004441 ) ;
#5103 = FACE_OUTER_BOUND ( 'NONE', #15295, .T. ) ;
#5104 = DIRECTION ( 'NONE',  ( -0.000000000000000000, -0.000000000000000000, -1.000000000000000000 ) ) ;
#5105 = CARTESIAN_POINT ( 'NONE',  ( -224.3206423881711089, 145.3335695535245975, -0.03206942349657965208 ) ) ;
#5106 = DIRECTION ( 'NONE',  ( 1.000000000000000000, 0.000000000000000000, 0.000000000000000000 ) ) ;
#5108 = VECTOR ( 'NONE', #931, 1000.000000000000000 ) ;
#5107 = AXIS2_PLACEMENT_3D ( 'NONE', #13496, #6577, #11379 ) ;
#5109 = DIRECTION ( 'NONE',  ( 1.000000000000000000, 0.000000000000000000, 0.000000000000000000 ) ) ;
#5110 = CARTESIAN_POINT ( 'NONE',  ( -178.4232521731099439, 131.0169814278324907, 7.919662025281895446 ) ) ;
#5111 = CARTESIAN_POINT ( 'NONE',  ( 122.5806775638430253, 45.00321902537314145, 9.975000000000001421 ) ) ;
#5112 = DIRECTION ( 'NONE',  ( 0.000000000000000000, -1.000000000000000000, -4.956352788505162775E-17 ) ) ;
#5113 = VERTEX_POINT ( 'NONE', #1495 ) ;
#5114 = CARTESIAN_POINT ( 'NONE',  ( 177.5000000000000853, -179.8058001507315566, 65.31842631998698323 ) ) ;
#5115 = ADVANCED_FACE ( 'NONE', ( #75 ), #6333, .F. ) ;
#5116 = ORIENTED_EDGE ( 'NONE', *, *, #7868, .F. ) ;
#5117 = ORIENTED_EDGE ( 'NONE', *, *, #9159, .F. ) ;
#5118 = CARTESIAN_POINT ( 'NONE',  ( 190.0000000000000568, -179.8058001507315566, -17.50000000000002487 ) ) ;
#5119 = DIRECTION ( 'NONE',  ( -0.000000000000000000, -0.000000000000000000, 1.000000000000000000 ) ) ;
#5120 = DIRECTION ( 'NONE',  ( 0.000000000000000000, 1.000000000000000000, 6.938893903907227145E-17 ) ) ;
#5121 = FILL_AREA_STYLE_COLOUR ( '', #4090 ) ;
#5122 = CARTESIAN_POINT ( 'NONE',  ( 0.2456200930618629430, 3.175426480542944407, 1.454290997841272695E-16 ) ) ;
#5123 = FACE_OUTER_BOUND ( 'NONE', #10624, .T. ) ;
#5124 = AXIS2_PLACEMENT_3D ( 'NONE', #10270, #4492, #619 ) ;
#5125 = CARTESIAN_POINT ( 'NONE',  ( 172.5293059057019889, 61.25683321636181233, 10.00000000000000178 ) ) ;
#5126 = CARTESIAN_POINT ( 'NONE',  ( -215.8266853215729668, 152.1588074852305112, 7.919662025281898998 ) ) ;
#5127 = ORIENTED_EDGE ( 'NONE', *, *, #12744, .T. ) ;
#5128 = DIRECTION ( 'NONE',  ( 0.000000000000000000, 0.000000000000000000, 1.000000000000000000 ) ) ;
#5129 = CARTESIAN_POINT ( 'NONE',  ( 208.8051451104704768, 39.65587490144260840, -4.559632177755815086 ) ) ;
#5130 = ADVANCED_FACE ( 'NONE', ( #4831 ), #10168, .T. ) ;
#5131 = DIRECTION ( 'NONE',  ( 0.000000000000000000, -1.000000000000000000, -1.156482317317871478E-16 ) ) ;
#5132 = ORIENTED_EDGE ( 'NONE', *, *, #12628, .F. ) ;
#5133 = AXIS2_PLACEMENT_3D ( 'NONE', #4880, #11987, #4559 ) ;
#5134 = CARTESIAN_POINT ( 'NONE',  ( -218.4292495602899749, 151.8671251436307159, 8.843529103934264057 ) ) ;
#5135 = ORIENTED_EDGE ( 'NONE', *, *, #10489, .T. ) ;
#5136 = CARTESIAN_POINT ( 'NONE',  ( -167.7990583880505824, 127.5943188236592363, 2.500000001005440620 ) ) ;
#5137 = CARTESIAN_POINT ( 'NONE',  ( 204.1086650545086911, 51.64708631006858752, -0.9236185576248838736 ) ) ;
#5139 = ORIENTED_EDGE ( 'NONE', *, *, #12205, .T. ) ;
#5138 = CIRCLE ( 'NONE', #4882, 3.525000000000000355 ) ;
#5140 = LINE ( 'NONE', #9966, #2637 ) ;
#5141 = CARTESIAN_POINT ( 'NONE',  ( 184.0000000000000568, 17.53993994372673271, 45.99999999999998579 ) ) ;
#5142 = EDGE_CURVE ( 'NONE', #8109, #13181, #12237, .T. ) ;
#5143 = CARTESIAN_POINT ( 'NONE',  ( -61.94838851346079167, -181.3058001507315566, 84.88378295107885663 ) ) ;
#5144 = ORIENTED_EDGE ( 'NONE', *, *, #765, .T. ) ;
#5145 = VECTOR ( 'NONE', #10010, 999.9999999999998863 ) ;
#5146 = APPLICATION_PROTOCOL_DEFINITION ( 'draft international standard', 'automotive_design', 1998, #785 ) ;
#5147 = EDGE_LOOP ( 'NONE', ( #10082, #3185, #6835, #4210 ) ) ;
#5148 = DIRECTION ( 'NONE',  ( 0.000000000000000000, 0.000000000000000000, -1.000000000000000000 ) ) ;
#5149 = DIRECTION ( 'NONE',  ( 1.000000000000000000, 0.000000000000000000, 0.000000000000000000 ) ) ;
#5150 = ORIENTED_EDGE ( 'NONE', *, *, #10337, .T. ) ;
#5151 = DIRECTION ( 'NONE',  ( -0.7071067811865425767, 0.000000000000000000, 0.7071067811865525687 ) ) ;
#5152 = EDGE_CURVE ( 'NONE', #4850, #5311, #6251, .T. ) ;
#5153 = DIRECTION ( 'NONE',  ( 0.000000000000000000, 0.000000000000000000, 1.000000000000000000 ) ) ;
#5154 = VERTEX_POINT ( 'NONE', #3642 ) ;
#5155 = ORIENTED_EDGE ( 'NONE', *, *, #7500, .F. ) ;
#5156 = CARTESIAN_POINT ( 'NONE',  ( -193.7200834347810599, 142.0619459586758921, 2.500000000000000000 ) ) ;
#5157 = CARTESIAN_POINT ( 'NONE',  ( 205.4081958545874613, 47.87064854543508829, -4.057643371672452481 ) ) ;
#5158 = ORIENTED_EDGE ( 'NONE', *, *, #8786, .F. ) ;
#5159 = FACE_OUTER_BOUND ( 'NONE', #4678, .T. ) ;
#5160 = DIRECTION ( 'NONE',  ( -1.000000000000000000, 0.000000000000000000, 0.000000000000000000 ) ) ;
#5161 = CARTESIAN_POINT ( 'NONE',  ( 10.39230484541326582, 0.000000000000000000, 5.000000000000000000 ) ) ;
#5162 = ADVANCED_FACE ( 'NONE', ( #8545 ), #9888, .T. ) ;
#5163 = CIRCLE ( 'NONE', #10970, 1.700000000000007061 ) ;
#5164 = CARTESIAN_POINT ( 'NONE',  ( -63.50000000000002842, 17.53993994372674692, -17.50000000000002487 ) ) ;
#5165 = CARTESIAN_POINT ( 'NONE',  ( 207.0901250877858217, 35.54806830018342367, -3.235595374952740855 ) ) ;
#5166 = EDGE_LOOP ( 'NONE', ( #15387, #11778 ) ) ;
#5167 = DIRECTION ( 'NONE',  ( 0.000000000000000000, -0.000000000000000000, 1.000000000000000000 ) ) ;
#5168 = CARTESIAN_POINT ( 'NONE',  ( -221.5309300683038032, 146.0635204735091293, -4.506196516310935429 ) ) ;
#5169 = CARTESIAN_POINT ( 'NONE',  ( -220.7908126485560274, 143.2766720833714089, -2.964974570226855288 ) ) ;
#5171 = EDGE_CURVE ( 'NONE', #11731, #9150, #4249, .T. ) ;
#5170 = DIRECTION ( 'NONE',  ( 0.000000000000000000, -1.000000000000000000, 0.000000000000000000 ) ) ;
#5172 = EDGE_CURVE ( 'NONE', #11790, #8811, #14910, .T. ) ;
#5173 = ORIENTED_EDGE ( 'NONE', *, *, #3106, .F. ) ;
#5174 = CARTESIAN_POINT ( 'NONE',  ( -173.9416064256852508, 115.8726071073731987, 1.253181679794994174 ) ) ;
#5175 = CARTESIAN_POINT ( 'NONE',  ( 194.8381067511959372, 47.88228248201940573, -3.436395123936771601 ) ) ;
#5176 = ORIENTED_EDGE ( 'NONE', *, *, #6734, .T. ) ;
#5177 = EDGE_LOOP ( 'NONE', ( #7110, #11271, #4443, #10831 ) ) ;
#5178 = EDGE_CURVE ( 'NONE', #7996, #5606, #6654, .T. ) ;
#5179 = AXIS2_PLACEMENT_3D ( 'NONE', #12020, #3575, #1121 ) ;
#5180 = PLANE ( 'NONE',  #1606 ) ;
#5181 = CARTESIAN_POINT ( 'NONE',  ( -70.00000000000000000, -181.3058001507315566, 74.95141194869098911 ) ) ;
#5182 = LINE ( 'NONE', #656, #4285 ) ;
#5183 = DIRECTION ( 'NONE',  ( 1.000000000000000000, 0.000000000000000000, 0.000000000000000000 ) ) ;
#5184 = DIRECTION ( 'NONE',  ( 3.965082230804130220E-16, 4.956352788505162775E-17, -1.000000000000000000 ) ) ;
#5185 = VECTOR ( 'NONE', #9258, 1000.000000000000114 ) ;
#5186 = ADVANCED_FACE ( 'NONE', ( #15059, #10267 ), #5374, .F. ) ;
#5187 = EDGE_CURVE ( 'NONE', #6271, #2702, #10927, .T. ) ;
#5188 = CARTESIAN_POINT ( 'NONE',  ( -206.0222741447286126, 148.9180917377961464, 3.478855109513426580 ) ) ;
#5189 = DIRECTION ( 'NONE',  ( -0.000000000000000000, -0.9902680687415712502, -0.1391731009600586100 ) ) ;
#5190 = CARTESIAN_POINT ( 'NONE',  ( -63.50000000000002842, 19.53993994372674692, -17.50000000000002487 ) ) ;
#5191 = EDGE_LOOP ( 'NONE', ( #896, #4973, #15325, #3038 ) ) ;
#5192 = AXIS2_PLACEMENT_3D ( 'NONE', #655, #5495, #3122 ) ;
#5193 = CARTESIAN_POINT ( 'NONE',  ( -63.50000000000002842, 19.53993994372673626, 52.49999999999997868 ) ) ;
#5194 = EDGE_LOOP ( 'NONE', ( #2103, #14481, #846, #7845 ) ) ;
#5195 = ORIENTED_EDGE ( 'NONE', *, *, #624, .F. ) ;
#5196 = DIRECTION ( 'NONE',  ( -0.000000000000000000, 1.000000000000000000, -0.000000000000000000 ) ) ;
#5197 = CARTESIAN_POINT ( 'NONE',  ( 0.000000000000000000, -6.928203230275514990, -4.000000000000003553 ) ) ;
#5198 = CARTESIAN_POINT ( 'NONE',  ( 65.70000000000004547, 62.13993994372673768, 15.00000000000070166 ) ) ;
#5199 = LINE ( 'NONE', #4003, #4199 ) ;
#5200 = CARTESIAN_POINT ( 'NONE',  ( -218.4373823716798597, 155.8743533890948356, 2.316433880752911012 ) ) ;
#5201 = CARTESIAN_POINT ( 'NONE',  ( -202.0760438715631437, 146.2294067514662288, 5.434754235172608361 ) ) ;
#5202 = ORIENTED_EDGE ( 'NONE', *, *, #534, .T. ) ;
#5203 = ADVANCED_FACE ( 'NONE', ( #3087 ), #9092, .T. ) ;
#5204 = AXIS2_PLACEMENT_3D ( 'NONE', #4555, #9382, #4395 ) ;
#5205 = CARTESIAN_POINT ( 'NONE',  ( -164.5262273476079713, 106.7842295329138835, 0.000000000000000000 ) ) ;
#5206 = UNCERTAINTY_MEASURE_WITH_UNIT (LENGTH_MEASURE( 1.000000000000000082E-05 ), #5727, 'distance_accuracy_value', 'NONE');
#5207 = CARTESIAN_POINT ( 'NONE',  ( 5.799999999999999822, -4.618802153517037823, -7.999999999999979572 ) ) ;
#5208 = CARTESIAN_POINT ( 'NONE',  ( -219.7781685404717393, 153.4721244997903398, 5.234562638556204739 ) ) ;
#5209 = VERTEX_POINT ( 'NONE', #5292 ) ;
#5210 = CARTESIAN_POINT ( 'NONE',  ( -220.6620190085783406, 151.8885676450574636, 7.148697176988450863 ) ) ;
#5211 = ORIENTED_EDGE ( 'NONE', *, *, #6054, .F. ) ;
#5212 = CARTESIAN_POINT ( 'NONE',  ( -169.2883314711424134, 124.9260523188610392, -3.943474352876168876 ) ) ;
#5213 = AXIS2_PLACEMENT_3D ( 'NONE', #9549, #14349, #2283 ) ;
#5214 = CARTESIAN_POINT ( 'NONE',  ( 207.2900793066480674, 50.33932807692791300, -4.067002334276190290 ) ) ;
#5215 = ORIENTED_EDGE ( 'NONE', *, *, #7718, .T. ) ;
#5216 = FACE_OUTER_BOUND ( 'NONE', #9265, .T. ) ;
#5217 = CARTESIAN_POINT ( 'NONE',  ( 0.7145311798163258565, 9.237604307034018802, 0.000000000000000000 ) ) ;
#5218 = ADVANCED_FACE ( 'NONE', ( #10346 ), #10117, .F. ) ;
#5219 = CARTESIAN_POINT ( 'NONE',  ( -64.00000000000002842, -178.8058001507315566, 52.69066787724494816 ) ) ;
#5220 = VERTEX_POINT ( 'NONE', #12700 ) ;
#5221 = CARTESIAN_POINT ( 'NONE',  ( 184.0000000000000568, 21.53993994372675758, 47.49999999999997868 ) ) ;
#5222 = ORIENTED_EDGE ( 'NONE', *, *, #6856, .T. ) ;
#5223 = CARTESIAN_POINT ( 'NONE',  ( 186.1005832062958234, 72.46888774096882457, 5.000000000000000000 ) ) ;
#5224 = DIRECTION ( 'NONE',  ( 0.000000000000000000, 0.000000000000000000, -1.000000000000000000 ) ) ;
#5225 = EDGE_LOOP ( 'NONE', ( #9851, #3463, #7929, #3011 ) ) ;
#5226 = FACE_OUTER_BOUND ( 'NONE', #9470, .T. ) ;
#5227 = DIRECTION ( 'NONE',  ( -1.000000000000000000, -2.751328491981765035E-32, 3.965082230804130220E-16 ) ) ;
#5228 = VERTEX_POINT ( 'NONE', #6493 ) ;
#5229 = VERTEX_POINT ( 'NONE', #3005 ) ;
#5230 = LINE ( 'NONE', #1674, #1459 ) ;
#5231 = CARTESIAN_POINT ( 'NONE',  ( 203.2140370934807834, 48.77700970988914264, -0.9247215889056725757 ) ) ;
#5232 = ORIENTED_EDGE ( 'NONE', *, *, #8793, .T. ) ;
#5233 = CARTESIAN_POINT ( 'NONE',  ( -205.9650630239422640, 131.2381394179032839, 2.431555724346861957 ) ) ;
#5234 = LINE ( 'NONE', #9114, #3280 ) ;
#5235 = CARTESIAN_POINT ( 'NONE',  ( -76.00000000000004263, -179.8058001507315566, 52.19066787724494816 ) ) ;
#5236 = CYLINDRICAL_SURFACE ( 'NONE', #8989, 3.499999999999999556 ) ;
#5237 = LINE ( 'NONE', #13755, #2521 ) ;
#5238 = VECTOR ( 'NONE', #11587, 1000.000000000000000 ) ;
#5239 = EDGE_LOOP ( 'NONE', ( #5753, #9600, #290, #3891 ) ) ;
#5240 = CYLINDRICAL_SURFACE ( 'NONE', #5078, 0.5000000000000004441 ) ;
#5241 = CARTESIAN_POINT ( 'NONE',  ( 2.000000000000000000, 0.000000000000000000, 1.499999999999999778 ) ) ;
#5242 = CIRCLE ( 'NONE', #13036, 1.000000000000000888 ) ;
#5243 = CARTESIAN_POINT ( 'NONE',  ( -198.4137021260360711, 129.4968702780754199, -2.964974570226842410 ) ) ;
#5244 = DIRECTION ( 'NONE',  ( 1.000000000000000000, 0.000000000000000000, 0.000000000000000000 ) ) ;
#5245 = ORIENTED_EDGE ( 'NONE', *, *, #6453, .F. ) ;
#5246 = CARTESIAN_POINT ( 'NONE',  ( -184.9748306402843809, 119.2867206268225999, 1.515400478619091995 ) ) ;
#5247 = CARTESIAN_POINT ( 'NONE',  ( 191.3907470605235801, 42.09736693221333326, -1.487451979171016125 ) ) ;
#5248 = ORIENTED_EDGE ( 'NONE', *, *, #998, .F. ) ;
#5249 = CARTESIAN_POINT ( 'NONE',  ( -61.94838851346079167, 15.53993994372673981, -2.500000000000070610 ) ) ;
#5250 = DIRECTION ( 'NONE',  ( 0.000000000000000000, -1.000000000000000000, -4.956352788505162775E-17 ) ) ;
#5251 =( GEOMETRIC_REPRESENTATION_CONTEXT ( 3 ) GLOBAL_UNCERTAINTY_ASSIGNED_CONTEXT ( ( #9162 ) ) GLOBAL_UNIT_ASSIGNED_CONTEXT ( ( #9211, #8032, #9442 ) ) REPRESENTATION_CONTEXT ( 'NONE', 'WORKASPACE' ) );
#5252 = DIRECTION ( 'NONE',  ( 0.8731965799097682890, -0.4873681696970819099, 0.000000000000000000 ) ) ;
#5253 = AXIS2_PLACEMENT_3D ( 'NONE', #7960, #12748, #8908 ) ;
#5254 = EDGE_CURVE ( 'NONE', #470, #11835, #11290, .T. ) ;
#5255 = B_SPLINE_CURVE_WITH_KNOTS ( 'NONE', 3,
 ( #1793, #6710, #14099, #13877, #6863, #11514, #3301, #756, #13953, #8136, #3213, #6780, #1942, #12921, #5596, #3141, #10406, #15275, #2989, #2108, #6942, #15351, #8051, #9072, #5514, #10250, #10485, #11674, #7971, #671, #11590, #3069, #12759, #599, #12681, #10330, #15201, #4234, #15043, #835, #15124, #10558, #9227, #12837, #7897, #5670, #4469, #1868, #5743, #11749 ),
 .UNSPECIFIED., .F., .F.,
 ( 4, 2, 2, 2, 2, 2, 2, 2, 2, 2, 2, 2, 2, 2, 2, 2, 2, 2, 2, 2, 2, 2, 2, 2, 4 ),
 ( 0.04400301569768626936, 0.04538375231244021896, 0.04676448892719416855, 0.04745485723457115029, 0.04814522554194812509, 0.04952596215670206081, 0.05021633046407901479, 0.05090669877145596878, 0.05228743538620987674, 0.05297780369358683072, 0.05366817200096378471, 0.05435854030834073175, 0.05504890861571768573, 0.05642964523047158676, 0.05712001353784854768, 0.05781038184522550166, 0.05850075015260245564, 0.05919111845997940963, 0.06057185507473332453, 0.06126222338211030627, 0.06195259168948728801, 0.06333332830424129312, 0.06471406491899528435, 0.06540443322637229384, 0.06609480153374930333 ),
 .UNSPECIFIED. ) ;
#5256 = CARTESIAN_POINT ( 'NONE',  ( 184.0000000000000568, 19.53993994372674337, -12.49999999999999467 ) ) ;
#5257 = VERTEX_POINT ( 'NONE', #9172 ) ;
#5258 = DIRECTION ( 'NONE',  ( -0.000000000000000000, 1.000000000000000000, -0.000000000000000000 ) ) ;
#5259 = CARTESIAN_POINT ( 'NONE',  ( -202.0760438715631437, 146.2294067514662288, 5.434754235172608361 ) ) ;
#5260 = CARTESIAN_POINT ( 'NONE',  ( 21.99999999999999289, 0.000000000000000000, 0.000000000000000000 ) ) ;
#5261 = LINE ( 'NONE', #9373, #2265 ) ;
#5262 = VERTEX_POINT ( 'NONE', #1884 ) ;
#5263 = LINE ( 'NONE', #5193, #12615 ) ;
#5264 = CIRCLE ( 'NONE', #191, 325.5619230110239073 ) ;
#5265 = ORIENTED_EDGE ( 'NONE', *, *, #1602, .F. ) ;
#5266 = VERTEX_POINT ( 'NONE', #9012 ) ;
#5267 = DIRECTION ( 'NONE',  ( 0.000000000000000000, 0.000000000000000000, -1.000000000000000000 ) ) ;
#5268 = CARTESIAN_POINT ( 'NONE',  ( 190.0000000000000568, 16.03993994372673981, 24.94742576086838781 ) ) ;
#5269 = LINE ( 'NONE', #2915, #7866 ) ;
#5270 = CARTESIAN_POINT ( 'NONE',  ( -99.68324453533686835, 80.15913712344708131, 5.000000000000000000 ) ) ;
#5271 = DIRECTION ( 'NONE',  ( 0.000000000000000000, 0.000000000000000000, 1.000000000000000000 ) ) ;
#5272 = CARTESIAN_POINT ( 'NONE',  ( -219.5883309621183628, 153.8122483208824463, -3.038090696635943999 ) ) ;
#5273 = EDGE_CURVE ( 'NONE', #10340, #8004, #6929, .T. ) ;
#5274 = EDGE_CURVE ( 'NONE', #9587, #5655, #11462, .T. ) ;
#5275 = ADVANCED_FACE ( 'NONE', ( #4333 ), #2934, .T. ) ;
#5276 = TOROIDAL_SURFACE ( 'NONE', #7309, 1.000000000000000000, 0.5000000000000000000 ) ;
#5277 = ORIENTED_EDGE ( 'NONE', *, *, #8268, .T. ) ;
#5278 = AXIS2_PLACEMENT_3D ( 'NONE', #10614, #15404, #14381 ) ;
#5279 = DIRECTION ( 'NONE',  ( -0.000000000000000000, -0.000000000000000000, 1.000000000000000000 ) ) ;
#5280 = DIRECTION ( 'NONE',  ( -0.000000000000000000, 1.000000000000000000, -0.000000000000000000 ) ) ;
#5281 = DIRECTION ( 'NONE',  ( 1.000000000000000000, 0.000000000000000000, 0.000000000000000000 ) ) ;
#5282 = CIRCLE ( 'NONE', #3774, 0.5000000000000004441 ) ;
#5283 = CARTESIAN_POINT ( 'NONE',  ( -70.00000000000000000, 19.53993994372673626, 48.99999999999997158 ) ) ;
#5284 = EDGE_LOOP ( 'NONE', ( #14887, #3856, #6417, #880 ) ) ;
#5285 = AXIS2_PLACEMENT_3D ( 'NONE', #5560, #9120, #479 ) ;
#5286 = CIRCLE ( 'NONE', #7321, 5.000000000000000000 ) ;
#5287 = CARTESIAN_POINT ( 'NONE',  ( -220.9667893534755194, 151.3425237312999911, 7.477333657888038942 ) ) ;
#5288 = ORIENTED_EDGE ( 'NONE', *, *, #11449, .T. ) ;
#5289 = DIRECTION ( 'NONE',  ( -0.4873681696970815769, -0.8731965799097684000, 0.000000000000000000 ) ) ;
#5290 = DIRECTION ( 'NONE',  ( -0.000000000000000000, 1.000000000000000000, -0.000000000000000000 ) ) ;
#5291 = ORIENTED_EDGE ( 'NONE', *, *, #10684, .T. ) ;
#5292 = CARTESIAN_POINT ( 'NONE',  ( -76.50000000000001421, 17.53993994372674692, -17.50000000000002487 ) ) ;
#5293 = FACE_OUTER_BOUND ( 'NONE', #12041, .T. ) ;
#5294 = AXIS2_PLACEMENT_3D ( 'NONE', #2456, #8623, #13421 ) ;
#5295 = CARTESIAN_POINT ( 'NONE',  ( -108.0000000000000568, 59.53993994372674337, 20.00000000000000355 ) ) ;
#5296 = ORIENTED_EDGE ( 'NONE', *, *, #6614, .F. ) ;
#5297 = AXIS2_PLACEMENT_3D ( 'NONE', #751, #34, #1223 ) ;
#5298 = ORIENTED_EDGE ( 'NONE', *, *, #8566, .F. ) ;
#5299 = CARTESIAN_POINT ( 'NONE',  ( -157.6233538794060962, 110.4504304370075829, 9.499964102291375667 ) ) ;
#5300 = EDGE_LOOP ( 'NONE', ( #14149, #444, #3207, #6306, #12153 ) ) ;
#5301 = CARTESIAN_POINT ( 'NONE',  ( -85.99999999999994316, 59.53993994372674337, 16.70000000000174012 ) ) ;
#5302 = EDGE_CURVE ( 'NONE', #12005, #13965, #8172, .T. ) ;
#5303 = DIRECTION ( 'NONE',  ( 0.000000000000000000, 0.000000000000000000, 1.000000000000000000 ) ) ;
#5304 = VECTOR ( 'NONE', #12314, 1000.000000000000114 ) ;
#5305 = EDGE_LOOP ( 'NONE', ( #3629, #13158, #9901, #5139 ) ) ;
#5306 = ORIENTED_EDGE ( 'NONE', *, *, #10203, .F. ) ;
#5307 = CARTESIAN_POINT ( 'NONE',  ( -172.3538414453648500, 130.1468270526879110, 1.515441478062062641 ) ) ;
#5308 = DIRECTION ( 'NONE',  ( 0.000000000000000000, -1.486905836551548832E-16, 1.000000000000000000 ) ) ;
#5309 = VECTOR ( 'NONE', #10690, 1000.000000000000000 ) ;
#5310 = EDGE_CURVE ( 'NONE', #6421, #4804, #14826, .T. ) ;
#5311 = VERTEX_POINT ( 'NONE', #375 ) ;
#5312 = AXIS2_PLACEMENT_3D ( 'NONE', #13935, #4451, #9135 ) ;
#5313 = CARTESIAN_POINT ( 'NONE',  ( 207.1164837741930569, 35.57719129110033407, -1.806778302941847159 ) ) ;
#5314 = CARTESIAN_POINT ( 'NONE',  ( 177.5000000000000853, -181.3058001507315566, 84.88378295107885663 ) ) ;
#5315 = CARTESIAN_POINT ( 'NONE',  ( -155.6477983077465410, 110.1970436846185066, -4.856732557889651858 ) ) ;
#5316 = LINE ( 'NONE', #1327, #6981 ) ;
#5317 = DIRECTION ( 'NONE',  ( -0.000000000000000000, 1.000000000000000000, -0.000000000000000000 ) ) ;
#5318 = AXIS2_PLACEMENT_3D ( 'NONE', #4462, #12987, #4308 ) ;
#5319 = LINE ( 'NONE', #9038, #11336 ) ;
#5320 = ORIENTED_EDGE ( 'NONE', *, *, #2331, .T. ) ;
#5321 = FACE_BOUND ( 'NONE', #15058, .T. ) ;
#5322 = DIRECTION ( 'NONE',  ( 0.9296197478520976665, 0.3660421972118349521, -0.04266420354037676888 ) ) ;
#5323 = CARTESIAN_POINT ( 'NONE',  ( -209.2730951545231335, 145.1348166524657302, -4.640918829492436615 ) ) ;
#5324 = DIRECTION ( 'NONE',  ( 3.965082230804130220E-16, 1.090924371466202084E-47, 1.000000000000000000 ) ) ;
#5325 = ORIENTED_EDGE ( 'NONE', *, *, #8305, .T. ) ;
#5326 = ADVANCED_FACE ( 'NONE', ( #5216 ), #8937, .T. ) ;
#5327 = CARTESIAN_POINT ( 'NONE',  ( -182.0950013669840359, 118.3955881831737997, 3.410453015226076801 ) ) ;
#5328 = CARTESIAN_POINT ( 'NONE',  ( 208.8002188652075972, 39.64064887424692785, -1.560527519332197022 ) ) ;
#5329 = VERTEX_POINT ( 'NONE', #12855 ) ;
#5330 = AXIS2_PLACEMENT_3D ( 'NONE', #11219, #13644, #7512 ) ;
#5331 = CARTESIAN_POINT ( 'NONE',  ( -151.4086188282879277, 107.2728346664360259, 0.000000000000000000 ) ) ;
#5332 = DIRECTION ( 'NONE',  ( 1.000000000000000000, 0.000000000000000000, 0.000000000000000000 ) ) ;
#5333 = AXIS2_PLACEMENT_3D ( 'NONE', #13680, #8890, #482 ) ;
#5334 = EDGE_CURVE ( 'NONE', #14252, #6288, #14183, .T. ) ;
#5335 = CARTESIAN_POINT ( 'NONE',  ( 190.5000000000000853, -178.9449732516916072, 64.32815825124538378 ) ) ;
#5336 = DIRECTION ( 'NONE',  ( 0.8731965799097690661, -0.4873681696970805222, 0.000000000000000000 ) ) ;
#5337 = EDGE_CURVE ( 'NONE', #5538, #14046, #7114, .T. ) ;
#5338 = ORIENTED_EDGE ( 'NONE', *, *, #6815, .T. ) ;
#5339 = VECTOR ( 'NONE', #12384, 1000.000000000000000 ) ;
#5340 = CYLINDRICAL_SURFACE ( 'NONE', #94, 1.699999999999994849 ) ;
#5341 = CARTESIAN_POINT ( 'NONE',  ( -187.9175675668324175, 138.8130845598205667, 3.478855109513427468 ) ) ;
#5342 = FACE_OUTER_BOUND ( 'NONE', #1738, .T. ) ;
#5343 = AXIS2_PLACEMENT_3D ( 'NONE', #8394, #13171, #8162 ) ;
#5344 = DIRECTION ( 'NONE',  ( 1.000000000000000000, 0.000000000000000000, 0.000000000000000000 ) ) ;
#5345 = ORIENTED_EDGE ( 'NONE', *, *, #3154, .F. ) ;
#5346 = CARTESIAN_POINT ( 'NONE',  ( -76.50000000000001421, -179.2362136002515172, -18.26098611522645498 ) ) ;
#5347 = ADVANCED_FACE ( 'NONE', ( #10501 ), #8203, .T. ) ;
#5348 = ORIENTED_EDGE ( 'NONE', *, *, #14711, .T. ) ;
#5349 = ORIENTED_EDGE ( 'NONE', *, *, #1926, .F. ) ;
#5350 = DIRECTION ( 'NONE',  ( 0.9620645606903813762, 0.2728218852358138546, 0.000000000000000000 ) ) ;
#5351 = CARTESIAN_POINT ( 'NONE',  ( 124.2806775638430281, 45.00321902537314145, 10.00000000000000178 ) ) ;
#5352 = DIRECTION ( 'NONE',  ( 0.000000000000000000, -1.000000000000000000, 0.000000000000000000 ) ) ;
#5353 =( LENGTH_UNIT ( ) NAMED_UNIT ( * ) SI_UNIT ( .MILLI., .METRE. ) );
#5354 = DIRECTION ( 'NONE',  ( 0.000000000000000000, 0.000000000000000000, -1.000000000000000000 ) ) ;
#5355 = STYLED_ITEM ( 'NONE', ( #4051 ), #10819 ) ;
#5356 = CARTESIAN_POINT ( 'NONE',  ( -216.7684744367785186, 154.7672370854363635, 0.8965377175049941139 ) ) ;
#5357 = CARTESIAN_POINT ( 'NONE',  ( 114.0000000000000568, 64.53993994372673626, 11.47500000000035136 ) ) ;
#5358 = MECHANICAL_DESIGN_GEOMETRIC_PRESENTATION_REPRESENTATION (  '', ( #15177 ), #12660 ) ;
#5359 = ORIENTED_EDGE ( 'NONE', *, *, #9809, .T. ) ;
#5360 = DIRECTION ( 'NONE',  ( -1.000000000000000000, 0.000000000000000000, 0.000000000000000000 ) ) ;
#5361 = CARTESIAN_POINT ( 'NONE',  ( -85.99999999999994316, 64.53993994372673626, 15.00000000000174794 ) ) ;
#5362 = EDGE_CURVE ( 'NONE', #14837, #10092, #5759, .T. ) ;
#5363 = DIRECTION ( 'NONE',  ( 1.000000000000000000, 2.751328491981765035E-32, -3.965082230804130220E-16 ) ) ;
#5364 = CARTESIAN_POINT ( 'NONE',  ( -219.4139989651374947, 154.1245914589817119, 2.346545548906505907 ) ) ;
#5365 = ORIENTED_EDGE ( 'NONE', *, *, #13754, .T. ) ;
#5366 = CARTESIAN_POINT ( 'NONE',  ( -216.7978016317474044, 154.7161345818039422, 4.230144757024230984 ) ) ;
#5368 = EDGE_CURVE ( 'NONE', #5616, #973, #13677, .T. ) ;
#5367 = PRODUCT_RELATED_PRODUCT_CATEGORY ( 'part', '', ( #5635 ) ) ;
#5369 = VERTEX_POINT ( 'NONE', #15524 ) ;
#5370 = EDGE_CURVE ( 'NONE', #9838, #3955, #9196, .T. ) ;
#5371 = CARTESIAN_POINT ( 'NONE',  ( -168.3799913776774133, 126.5534861816458800, -1.907514191769585921 ) ) ;
#5372 = CARTESIAN_POINT ( 'NONE',  ( 14.00000000000004086, 59.53993994372674337, 15.00000000000104983 ) ) ;
#5373 = VERTEX_POINT ( 'NONE', #5686 ) ;
#5374 = PLANE ( 'NONE',  #8946 ) ;
#5375 = DIRECTION ( 'NONE',  ( -0.000000000000000000, 1.000000000000000000, -0.000000000000000000 ) ) ;
#5376 = EDGE_CURVE ( 'NONE', #4947, #7984, #3230, .T. ) ;
#5377 = PRODUCT_DEFINITION_SHAPE ( 'NONE', 'NONE',  #15628 ) ;
#5378 = VECTOR ( 'NONE', #451, 1000.000000000000000 ) ;
#5379 = DIRECTION ( 'NONE',  ( 1.000000000000000000, 0.000000000000000000, 0.000000000000000000 ) ) ;
#5380 = ORIENTED_EDGE ( 'NONE', *, *, #10076, .F. ) ;
#5381 = ITEM_DEFINED_TRANSFORMATION ( 'NONE', 'NONE', #10823,  #12337 ) ;
#5382 = ORIENTED_EDGE ( 'NONE', *, *, #791, .T. ) ;
#5383 = AXIS2_PLACEMENT_3D ( 'NONE', #8691, #5279, #204 ) ;
#5384 = CARTESIAN_POINT ( 'NONE',  ( -155.6738846654525048, 110.4594052389692962, 9.769471784547329563 ) ) ;
#5385 = ORIENTED_EDGE ( 'NONE', *, *, #5899, .T. ) ;
#5386 = CARTESIAN_POINT ( 'NONE',  ( -64.00000000000002842, -179.3058001507315566, -51.45141194869120227 ) ) ;
#5387 = ADVANCED_FACE ( 'NONE', ( #5839 ), #1959, .F. ) ;
#5388 =( GEOMETRIC_REPRESENTATION_CONTEXT ( 3 ) GLOBAL_UNCERTAINTY_ASSIGNED_CONTEXT ( ( #6756 ) ) GLOBAL_UNIT_ASSIGNED_CONTEXT ( ( #5353, #4156, #12680 ) ) REPRESENTATION_CONTEXT ( 'NONE', 'WORKASPACE' ) );
#5389 = CARTESIAN_POINT ( 'NONE',  ( 164.0000000000000568, 59.53993994372674337, 15.00000000000000355 ) ) ;
#5390 = ORIENTED_EDGE ( 'NONE', *, *, #6228, .F. ) ;
#5391 = ORIENTED_EDGE ( 'NONE', *, *, #1187, .T. ) ;
#5392 = CARTESIAN_POINT ( 'NONE',  ( -172.3582205330567945, 130.1389812296867774, 2.500000000525777644 ) ) ;
#5393 = CARTESIAN_POINT ( 'NONE',  ( -217.6896908598658911, 153.1102862775958897, 3.058976617611858906 ) ) ;
#5394 = ORIENTED_EDGE ( 'NONE', *, *, #1764, .T. ) ;
#5395 = CARTESIAN_POINT ( 'NONE',  ( 198.9111841706756536, 32.15857605477618364, -5.308824953579920347 ) ) ;
#5396 = CYLINDRICAL_SURFACE ( 'NONE', #1252, 54.67486482576605766 ) ;
#5397 = AXIS2_PLACEMENT_3D ( 'NONE', #4322, #13962, #3145 ) ;
#5398 = EDGE_CURVE ( 'NONE', #13381, #9509, #6124, .T. ) ;
#5399 = PLANE ( 'NONE',  #737 ) ;
#5400 = CARTESIAN_POINT ( 'NONE',  ( 184.0000000000000568, 15.53993994372673626, 48.99999999999997158 ) ) ;
#5401 = DIRECTION ( 'NONE',  ( 0.9296197478520976665, 0.3660421972118349521, -0.04266420354037676888 ) ) ;
#5402 = VECTOR ( 'NONE', #5027, 1000.000000000000000 ) ;
#5403 = EDGE_CURVE ( 'NONE', #14746, #14786, #4647, .T. ) ;
#5404 = CARTESIAN_POINT ( 'NONE',  ( -76.00000000000007105, -178.8058001507315566, 65.31842631998698323 ) ) ;
#5405 = ORIENTED_EDGE ( 'NONE', *, *, #1989, .T. ) ;
#5406 = DIRECTION ( 'NONE',  ( 0.000000000000000000, 0.000000000000000000, 1.000000000000000000 ) ) ;
#5407 = AXIS2_PLACEMENT_3D ( 'NONE', #1664, #5602, #15131 ) ;
#5408 = CARTESIAN_POINT ( 'NONE',  ( -171.9495551447802200, 125.1641050887067053, -4.702677209512893697 ) ) ;
#5409 = DIRECTION ( 'NONE',  ( 3.965082230804130220E-16, 1.090924371466202084E-47, 1.000000000000000000 ) ) ;
#5410 = ORIENTED_EDGE ( 'NONE', *, *, #346, .F. ) ;
#5411 = CARTESIAN_POINT ( 'NONE',  ( -178.4228374502453107, 119.2657932277225967, 7.804961498744191317 ) ) ;
#5412 = CARTESIAN_POINT ( 'NONE',  ( 201.7406124912899941, 52.65652330452660834, -2.244206067705167396 ) ) ;
#5413 = AXIS2_PLACEMENT_3D ( 'NONE', #13972, #3158, #11221 ) ;
#5414 = ORIENTED_EDGE ( 'NONE', *, *, #1087, .T. ) ;
#5415 = DIRECTION ( 'NONE',  ( -0.000000000000000000, -0.9902680687415713612, 0.1391731009600582492 ) ) ;
#5416 = CARTESIAN_POINT ( 'NONE',  ( 7.165898733771380869E-16, -0.2686526913948933948, 2.750000000000000888 ) ) ;
#5417 = CARTESIAN_POINT ( 'NONE',  ( 190.0000000000000568, 15.03993994372673981, -3.075184203610571654 ) ) ;
#5418 = CIRCLE ( 'NONE', #10468, 0.5000000000000004441 ) ;
#5419 = SHAPE_REPRESENTATION ( 'Recoil spring', ( #12337 ), #6298 ) ;
#5420 = CARTESIAN_POINT ( 'NONE',  ( 195.1062858801516597, 40.86394065090267702, 16.00000000000001421 ) ) ;
#5421 = EDGE_CURVE ( 'NONE', #10430, #6332, #601, .T. ) ;
#5422 = ORIENTED_EDGE ( 'NONE', *, *, #10755, .F. ) ;
#5423 = DIRECTION ( 'NONE',  ( 0.000000000000000000, 0.000000000000000000, -1.000000000000000000 ) ) ;
#5424 = CARTESIAN_POINT ( 'NONE',  ( -168.3973611425364822, 125.8284172634911755, 7.880738923213935543 ) ) ;
#5425 = DIRECTION ( 'NONE',  ( 0.000000000000000000, -1.486905836551548832E-16, 1.000000000000000000 ) ) ;
#5426 = DIRECTION ( 'NONE',  ( -1.000000000000000000, -0.000000000000000000, -0.000000000000000000 ) ) ;
#5427 = ORIENTED_EDGE ( 'NONE', *, *, #13085, .F. ) ;
#5428 = CARTESIAN_POINT ( 'NONE',  ( 170.2980342783642982, 56.44038842094546737, -0.9107274384406883749 ) ) ;
#5429 = AXIS2_PLACEMENT_3D ( 'NONE', #3039, #12804, #5406 ) ;
#5430 = VERTEX_POINT ( 'NONE', #10423 ) ;
#5431 = ORIENTED_EDGE ( 'NONE', *, *, #6089, .F. ) ;
#5432 = CARTESIAN_POINT ( 'NONE',  ( -150.8011781171663017, 108.0782419600532620, 9.825479475539731666 ) ) ;
#5433 = FACE_OUTER_BOUND ( 'NONE', #6447, .T. ) ;
#5434 = FILL_AREA_STYLE ('',( #6633 ) ) ;
#5435 = CARTESIAN_POINT ( 'NONE',  ( 178.0000000000000853, -179.8058001507315566, 52.19066787724494816 ) ) ;
#5436 = CARTESIAN_POINT ( 'NONE',  ( -220.2506544536004469, 152.6255918186425617, -1.607790317125668222 ) ) ;
#5437 = CARTESIAN_POINT ( 'NONE',  ( 169.5018791832601721, 101.0521538385604003, 0.000000000000000000 ) ) ;
#5438 = MANIFOLD_SOLID_BREP ( 'Cut-Extrude3', #11920 ) ;
#5439 = AXIS2_PLACEMENT_3D ( 'NONE', #13349, #2551, #1427 ) ;
#5440 = EDGE_CURVE ( 'NONE', #13575, #11344, #10452, .T. ) ;
#5441 = CARTESIAN_POINT ( 'NONE',  ( 190.0000000000000853, -179.3058001507316419, 52.76585208085545986 ) ) ;
#5442 = CARTESIAN_POINT ( 'NONE',  ( 122.5806775638430253, 45.00321902537314145, 7.600000000000002309 ) ) ;
#5443 = EDGE_CURVE ( 'NONE', #8472, #4749, #125, .T. ) ;
#5444 = AXIS2_PLACEMENT_3D ( 'NONE', #322, #5160, #161 ) ;
#5445 = CARTESIAN_POINT ( 'NONE',  ( 177.5000000000000853, -179.8058001507315566, 52.19066787724494816 ) ) ;
#5446 = CARTESIAN_POINT ( 'NONE',  ( -219.6200563868712266, 153.7554072423868661, 0.2735799752493159875 ) ) ;
#5447 = ORIENTED_EDGE ( 'NONE', *, *, #14332, .F. ) ;
#5448 = CARTESIAN_POINT ( 'NONE',  ( -219.2006734968679211, 154.5067975218504444, 7.020207066939610385 ) ) ;
#5449 = ORIENTED_EDGE ( 'NONE', *, *, #7116, .F. ) ;
#5450 = CARTESIAN_POINT ( 'NONE',  ( 190.0000000000000568, 15.53993994372673981, 10.05257423913146475 ) ) ;
#5451 = FACE_OUTER_BOUND ( 'NONE', #8279, .T. ) ;
#5452 = VECTOR ( 'NONE', #6639, 1000.000000000000000 ) ;
#5453 = EDGE_LOOP ( 'NONE', ( #4999, #10246 ) ) ;
#5454 = CARTESIAN_POINT ( 'NONE',  ( -61.94838851346079167, -179.3058001507315566, -51.45141194869120227 ) ) ;
#5455 = CARTESIAN_POINT ( 'NONE',  ( 114.0000000000000568, 64.51493994372674479, 15.00000000000035172 ) ) ;
#5456 = AXIS2_PLACEMENT_3D ( 'NONE', #12720, #1910, #712 ) ;
#5457 = EDGE_CURVE ( 'NONE', #14894, #9501, #851, .T. ) ;
#5458 = CARTESIAN_POINT ( 'NONE',  ( -151.4086188282879277, 107.2728346664360259, -5.000000000000000000 ) ) ;
#5459 = ORIENTED_EDGE ( 'NONE', *, *, #622, .F. ) ;
#5460 = EDGE_CURVE ( 'NONE', #4643, #3604, #3624, .T. ) ;
#5461 = B_SPLINE_CURVE_WITH_KNOTS ( 'NONE', 3,
 ( #10424, #10900, #13163, #2362, #7271, #2520 ),
 .UNSPECIFIED., .F., .F.,
 ( 4, 2, 4 ),
 ( 0.004557243715295504136, 0.005361529354039402256, 0.006165814992783300377 ),
 .UNSPECIFIED. ) ;
#5462 = ORIENTED_EDGE ( 'NONE', *, *, #10682, .F. ) ;
#5463 = CARTESIAN_POINT ( 'NONE',  ( 211.8964099132376191, 42.41229301046570299, -5.872780407435223893 ) ) ;
#5464 = ADVANCED_FACE ( 'NONE', ( #54 ), #4892, .T. ) ;
#5465 = EDGE_CURVE ( 'NONE', #8637, #1780, #13240, .T. ) ;
#5466 = DIRECTION ( 'NONE',  ( 0.000000000000000000, 0.000000000000000000, 1.000000000000000000 ) ) ;
#5467 = ORIENTED_EDGE ( 'NONE', *, *, #4300, .F. ) ;
#5468 = AXIS2_PLACEMENT_3D ( 'NONE', #13477, #6315, #5271 ) ;
#5469 = PLANE ( 'NONE',  #12491 ) ;
#5470 = CIRCLE ( 'NONE', #6222, 7.499999999999999112 ) ;
#5471 = DIRECTION ( 'NONE',  ( 1.000000000000000000, 0.000000000000000000, 0.000000000000000000 ) ) ;
#5472 = ORIENTED_EDGE ( 'NONE', *, *, #12782, .F. ) ;
#5473 = VERTEX_POINT ( 'NONE', #11045 ) ;
#5474 = CARTESIAN_POINT ( 'NONE',  ( 114.0000000000000568, 64.51493994372674479, 11.50000000000034817 ) ) ;
#5475 = DIRECTION ( 'NONE',  ( 0.000000000000000000, -1.000000000000000000, -6.938893903907227145E-17 ) ) ;
#5476 = ORIENTED_EDGE ( 'NONE', *, *, #15398, .T. ) ;
#5477 = CARTESIAN_POINT ( 'NONE',  ( 207.1167095084715868, 46.15093117762712893, -7.185265714380067337 ) ) ;
#5478 = DIRECTION ( 'NONE',  ( 0.000000000000000000, -1.000000000000000000, 0.000000000000000000 ) ) ;
#5479 = CARTESIAN_POINT ( 'NONE',  ( 6.399999999999999467, 4.618802153516981868, 8.000000000000007105 ) ) ;
#5480 = CARTESIAN_POINT ( 'NONE',  ( -70.00000000000000000, 17.53993994372673271, 47.49999999999997868 ) ) ;
#5481 = DIRECTION ( 'NONE',  ( 0.000000000000000000, 0.000000000000000000, -1.000000000000000000 ) ) ;
#5482 = EDGE_CURVE ( 'NONE', #9708, #7691, #5568, .T. ) ;
#5483 = EDGE_CURVE ( 'NONE', #3488, #7175, #3866, .T. ) ;
#5484 = DIRECTION ( 'NONE',  ( 0.000000000000000000, -0.5000000000000012212, 0.8660254037844380415 ) ) ;
#5485 = EDGE_LOOP ( 'NONE', ( #14630, #10433 ) ) ;
#5486 = DIRECTION ( 'NONE',  ( -0.3662838836490099337, 0.9305003370641709015, 0.002288952263120960697 ) ) ;
#5487 = CARTESIAN_POINT ( 'NONE',  ( -207.0700983879231387, 149.0508413170868209, -0.4547266291960758156 ) ) ;
#5488 = CARTESIAN_POINT ( 'NONE',  ( -151.4086188282879277, 107.2728346664360259, 5.000000000000000000 ) ) ;
#5489 = ORIENTED_EDGE ( 'NONE', *, *, #11728, .F. ) ;
#5490 = CARTESIAN_POINT ( 'NONE',  ( -225.7548303624725179, 142.7639966680278576, 3.410453015226076801 ) ) ;
#5491 = CARTESIAN_POINT ( 'NONE',  ( 203.7958462291278749, 29.94547861640233322, -6.526400227122580944 ) ) ;
#5492 = EDGE_LOOP ( 'NONE', ( #6776, #541, #4618, #11953 ) ) ;
#5493 = EDGE_CURVE ( 'NONE', #10896, #11184, #13429, .T. ) ;
#5494 = CARTESIAN_POINT ( 'NONE',  ( 202.1731860119849102, 31.08132011834958419, -8.150590381057213563 ) ) ;
#5495 = DIRECTION ( 'NONE',  ( -1.000000000000000000, -0.000000000000000000, -0.000000000000000000 ) ) ;
#5496 = CARTESIAN_POINT ( 'NONE',  ( 176.0293059057019889, 61.25683321636181233, 9.975000000000001421 ) ) ;
#5497 = CIRCLE ( 'NONE', #12565, 0.5000000000000001110 ) ;
#5498 = DIRECTION ( 'NONE',  ( -0.000000000000000000, 1.000000000000000000, -0.000000000000000000 ) ) ;
#5499 = ORIENTED_EDGE ( 'NONE', *, *, #14232, .T. ) ;
#5500 = CARTESIAN_POINT ( 'NONE',  ( -177.0244624812495999, 127.4802545373068767, 9.556866313350486308 ) ) ;
#5501 = DIRECTION ( 'NONE',  ( 0.000000000000000000, 0.000000000000000000, 1.000000000000000000 ) ) ;
#5502 = CARTESIAN_POINT ( 'NONE',  ( -155.6477983077465410, 110.1970436846185066, -4.856732557889651858 ) ) ;
#5503 = B_SPLINE_SURFACE_WITH_KNOTS ( 'NONE', 3, 3, ( 
 ( #5986, #13230, #4883, #2430, #1000, #9702, #1316, #13074, #11989, #13152, #14567, #4959, #9774, #7025, #11832, #10649, #9466 ),
 ( #1549, #14727, #6384, #11192, #5188, #13467, #500, #3989, #2904, #5341, #7727, #14796, #11268, #13536, #8823, #1385, #10085 ),
 ( #271, #6299, #5034, #13701, #2667, #5259, #11116, #13618, #7485, #2825, #12279, #7647, #12439, #14878, #12514, #4073, #3922 ),
 ( #6540, #6223, #10163, #14955, #9860, #8745, #9936, #4146, #14652, #3853, #1460, #8674, #5110, #2742, #7565, #15262, #5424 ),
 ( #3202, #824, #11575, #9143, #4458, #9290, #12747, #8037, #10545, #11504, #14087, #15032, #15111, #5500, #742, #11663, #6931 ),
 ( #6851, #1856, #10317, #7886, #3288, #7805, #5733, #12909, #10395, #661, #6621, #11420, #12825, #5658, #4303, #8122, #1932 ),
 ( #13941, #13779, #2013, #2098, #3128, #6699, #12668, #7959, #10475, #11738, #4221, #901, #586, #5584, #9059, #13865, #4544 ),
 ( #15340, #15189, #4384, #2976, #12592, #6768, #1782, #9215, #10240, #3057, #14012, #4621, #15499, #12039, #5889, #2251, #12116 ),
 ( #7168, #10707, #10948, #9449, #8433, #10871, #3670, #1295, #10786, #15573, #11971, #9371, #9519, #3516, #13212, #2410, #4696 ),
 ( #13049, #4778, #99, #2173, #5809, #13288, #8204, #13134, #14317, #14399, #1212, #8353, #14244, #2336, #14167, #3365, #6128 ),
 ( #1140, #10629, #15421, #5967, #1066, #7086, #12983, #6050, #3440, #9603, #3597, #7245, #4863, #7320, #7003, #8273, #11891 ),
 ( #25, #11813, #9682, #978, #14475, #8504, #2488, #11178, #8892, #6445, #12190, #13682, #9998, #7630, #2725, #254, #11250 ),
 ( #9759, #5169, #7549, #2888, #7711, #8654, #12346, #14549, #5243, #14781, #3751, #13450, #1370, #4939, #5018, #2570, #13601 ),
 ( #12497, #14861, #14708, #1531, #2809, #330, #8579, #6367, #3974, #6208, #5094, #14637, #1687, #9843, #11019, #7470, #13523 ),
 ( #13372, #9918, #3906, #8806, #12422, #1444, #1614, #2649, #406, #11324, #7400, #170, #6524, #3835, #8729, #6283, #10068 ),
 ( #4056, #12265, #11099, #5323, #6909, #3265, #8106, #4284, #1767, #6603, #647, #7870, #9042, #485, #8018, #5408, #722 ),
 ( #6684, #11643, #14072, #12890, #10224, #570, #2076, #11487, #14941, #15018, #4205, #11559, #9124, #3188, #11404, #805, #12728 ),
 ( #4441, #10377, #15245, #5487, #15092, #12806, #13997, #9275, #10148, #9201, #13842, #12653, #3040, #5639, #4131, #8970, #13763 ),
 ( #1840, #2961, #7786, #15170, #1995, #10301, #10458, #13925, #12570, #3114, #7944, #4365, #6832, #1917, #6752, #5565, #2231 ),
 ( #3651, #13116, #2315, #14297, #11720, #11875, #5872, #15552, #10766, #8256, #11951, #15403, #7145, #2465, #4521, #8182, #6 ) ),
 .UNSPECIFIED., .T., .F., .F.,
 ( 4, 1, 1, 1, 1, 1, 1, 1, 2, 1, 1, 1, 1, 1, 1, 1, 4 ),
 ( 4, 2, 2, 2, 2, 2, 3, 4 ),
 ( 0.000000000000000000, 0.06231844716590150685, 0.1246368943318030137, 0.1869553414977045136, 0.2492737886636060274, 0.3115922358295075134, 0.3739106829954090272, 0.4362291301613105410, 0.4985475773272120548, 0.5612291301613105965, 0.6239106829954090827, 0.6865922358295075689, 0.7492737886636060551, 0.8119553414977045414, 0.8746368943318030276, 0.9373184471659015138, 1.000000000000000000 ),
 ( 0.000000000000000000, 0.2455027589669699362, 0.3041813370740077405, 0.5308033955276700855, 0.6372805264318514018, 0.8233339832829627003, 1.000000000000000000, 1.166726064904226812 ),
 .UNSPECIFIED. ) ;
#5504 = VERTEX_POINT ( 'NONE', #1395 ) ;
#5505 = DIRECTION ( 'NONE',  ( 0.000000000000000000, 0.000000000000000000, -1.000000000000000000 ) ) ;
#5506 = VECTOR ( 'NONE', #12919, 1000.000000000000114 ) ;
#5507 = EDGE_LOOP ( 'NONE', ( #6972, #11279, #14787, #7265 ) ) ;
#5508 = ADVANCED_FACE ( 'NONE', ( #7270 ), #14502, .T. ) ;
#5509 = ORIENTED_EDGE ( 'NONE', *, *, #6344, .F. ) ;
#5510 = DIRECTION ( 'NONE',  ( 0.8731965799097686221, -0.4873681696970812438, -0.000000000000000000 ) ) ;
#5511 = CARTESIAN_POINT ( 'NONE',  ( 19.11029453487719110, 40.04259805664093363, 10.00000000000000178 ) ) ;
#5512 =( BOUNDED_SURFACE ( )  B_SPLINE_SURFACE ( 3, 2, ( 
 ( #2918, #4158, #6554 ),
 ( #3070, #358, #517 ),
 ( #6475, #5200, #15125 ),
 ( #7898, #12525, #4005 ),
 ( #5356, #2990, #10025 ),
 ( #10176, #13633, #11355 ),
 ( #6637, #13791, #10331 ),
 ( #10100, #7819, #11206 ),
 ( #7741, #600, #12682 ),
 ( #11278, #14966, #2838 ),
 ( #9156, #13954, #12608 ),
 ( #1794, #1716, #14893 ),
 ( #1869, #5272, #5436 ),
 ( #10251, #6711, #4316 ),
 ( #4089, #8920, #3142 ),
 ( #7659, #15044, #11515 ),
 ( #672, #5515, #12454 ),
 ( #7972, #6399, #5900 ),
 ( #1078, #12922, #914 ),
 ( #15433, #10719, #6782 ),
 ( #5671, #9305, #11675 ),
 ( #14101, #15352, #2109 ),
 ( #14258, #11591, #11750 ),
 ( #12840, #757, #15512 ),
 ( #8137, #1943, #992 ),
 ( #6943, #10486, #836 ),
 ( #9461, #5822, #3214 ),
 ( #4396, #9383, #8052 ),
 ( #8366, #4710, #11903 ),
 ( #4557, #3529, #5597 ),
 ( #11826, #5744, #4632 ),
 ( #9532, #14330, #10559 ),
 ( #3454, #12994, #10407 ),
 ( #14178, #9228, #3376 ),
 ( #15202, #6864, #14025 ),
 ( #8216, #2029, #15276 ),
 ( #2186, #3302, #7014 ),
 ( #10641, #4470, #8285 ),
 ( #13064, #2266, #7098 ),
 ( #14648, #7481, #5105 ),
 ( #14561, #112, #13146 ),
 ( #9697, #12132, #6141 ),
 ( #8444, #6293, #3765 ),
 ( #2501, #8516, #9931 ),
 ( #13302, #1308, #2348 ),
 ( #8592, #10884, #1228 ) ),
 .UNSPECIFIED., .F., .F., .T. ) 
 B_SPLINE_SURFACE_WITH_KNOTS ( ( 4, 2, 2, 2, 2, 2, 2, 2, 2, 2, 2, 2, 2, 2, 2, 2, 2, 2, 2, 2, 2, 2, 4 ),
 ( 3, 3 ),
 ( 0.01690353391188639809, 0.01796000478138011502, 0.01901647565087383543, 0.02007294652036755583, 0.02112941738986127277, 0.02165765282460813124, 0.02218588825935499317, 0.02324235912884871358, 0.02429882999834243051, 0.02482706543308928898, 0.02535530086783615092, 0.02641177173732987132, 0.02694000717207672979, 0.02746824260682358826, 0.02799647804157044673, 0.02852471347631730866, 0.02958118434581102907, 0.03010941978055788754, 0.03063765521530474600, 0.03169412608479846294, 0.03222236151954532141, 0.03275059695429217987, 0.03380706782378590375 ),
 ( 0.000000000000000000, 1.000000000000000000 ),
 .UNSPECIFIED. ) 
 GEOMETRIC_REPRESENTATION_ITEM ( )  RATIONAL_B_SPLINE_SURFACE ( (
 ( 1.000000000000000000, 0.7072571230116134755, 1.000000000000000000),
 ( 1.000000000000000000, 0.7070704586539242609, 1.000000000000000000),
 ( 1.000000000000000000, 0.7070624175750332974, 1.000000000000000000),
 ( 1.000000000000000000, 0.7073610487233381594, 1.000000000000000000),
 ( 1.000000000000000000, 0.7076621214645069102, 1.000000000000000000),
 ( 1.000000000000000000, 0.7084745963449632367, 1.000000000000000000),
 ( 1.000000000000000000, 0.7089917081225262097, 1.000000000000000000),
 ( 1.000000000000000000, 0.7100509560662205955, 1.000000000000000000),
 ( 1.000000000000000000, 0.7105995507477381734, 1.000000000000000000),
 ( 1.000000000000000000, 0.7113270099474451325, 1.000000000000000000),
 ( 1.000000000000000000, 0.7115528126308224843, 1.000000000000000000),
 ( 1.000000000000000000, 0.7119351551072216067, 1.000000000000000000),
 ( 1.000000000000000000, 0.7120930000513538971, 1.000000000000000000),
 ( 1.000000000000000000, 0.7124440185857547903, 1.000000000000000000),
 ( 1.000000000000000000, 0.7125154292520059496, 1.000000000000000000),
 ( 1.000000000000000000, 0.7121332859195406151, 1.000000000000000000),
 ( 1.000000000000000000, 0.7116646334020431119, 1.000000000000000000),
 ( 1.000000000000000000, 0.7105288043779220963, 1.000000000000000000),
 ( 1.000000000000000000, 0.7100784943464703014, 1.000000000000000000),
 ( 1.000000000000000000, 0.7090174157212792982, 1.000000000000000000),
 ( 1.000000000000000000, 0.7084074433244883506, 1.000000000000000000),
 ( 1.000000000000000000, 0.7063588986342012044, 1.000000000000000000),
 ( 1.000000000000000000, 0.7046589198606203475, 1.000000000000000000),
 ( 1.000000000000000000, 0.7017665165854515275, 1.000000000000000000),
 ( 1.000000000000000000, 0.7007370448553386089, 1.000000000000000000),
 ( 1.000000000000000000, 0.6986007619009740877, 1.000000000000000000),
 ( 1.000000000000000000, 0.6974911578170575055, 1.000000000000000000),
 ( 1.000000000000000000, 0.6951922021189940182, 1.000000000000000000),
 ( 1.000000000000000000, 0.6940027630648812895, 1.000000000000000000),
 ( 1.000000000000000000, 0.6915472827938593525, 1.000000000000000000),
 ( 1.000000000000000000, 0.6902979293261688465, 1.000000000000000000),
 ( 1.000000000000000000, 0.6865737038807442350, 1.000000000000000000),
 ( 1.000000000000000000, 0.6841432992373190913, 1.000000000000000000),
 ( 1.000000000000000000, 0.6806030716582376350, 1.000000000000000000),
 ( 1.000000000000000000, 0.6794407469212847550, 1.000000000000000000),
 ( 1.000000000000000000, 0.6771618041792656362, 1.000000000000000000),
 ( 1.000000000000000000, 0.6760782311690274327, 1.000000000000000000),
 ( 1.000000000000000000, 0.6730262767741563845, 1.000000000000000000),
 ( 1.000000000000000000, 0.6712352064082731662, 1.000000000000000000),
 ( 1.000000000000000000, 0.6689250498628499519, 1.000000000000000000),
 ( 1.000000000000000000, 0.6682166586818782950, 1.000000000000000000),
 ( 1.000000000000000000, 0.6669646655643757249, 1.000000000000000000),
 ( 1.000000000000000000, 0.6664264744289446485, 1.000000000000000000),
 ( 1.000000000000000000, 0.6650728498231318619, 1.000000000000000000),
 ( 1.000000000000000000, 0.6645102704218179834, 1.000000000000000000),
 ( 1.000000000000000000, 0.6642977373962596355, 1.000000000000000000) ) ) 
 REPRESENTATION_ITEM ( '' )  SURFACE ( )  );
#5513 = CARTESIAN_POINT ( 'NONE',  ( 6.399999999999999467, 4.618802153516981868, -7.999999999999979572 ) ) ;
#5514 = CARTESIAN_POINT ( 'NONE',  ( -171.2229998886518274, 121.4597901571797252, 9.827342307218824402 ) ) ;
#5515 = CARTESIAN_POINT ( 'NONE',  ( -220.6713114466640207, 151.8719187835573052, -4.501197839774258469 ) ) ;
#5516 = CYLINDRICAL_SURFACE ( 'NONE', #2681, 10.00000000000000888 ) ;
#5517 = VECTOR ( 'NONE', #12410, 1000.000000000000114 ) ;
#5518 = CARTESIAN_POINT ( 'NONE',  ( 190.0000000000000568, 15.53993994372673804, 25.38206912977649310 ) ) ;
#5519 = CARTESIAN_POINT ( 'NONE',  ( -108.0000000000000568, 59.53993994372674337, 20.00000000000000355 ) ) ;
#5520 = DIRECTION ( 'NONE',  ( -0.000000000000000000, 0.000000000000000000, 1.000000000000000000 ) ) ;
#5521 = DIRECTION ( 'NONE',  ( 0.000000000000000000, 1.000000000000000000, 0.000000000000000000 ) ) ;
#5522 = CIRCLE ( 'NONE', #13827, 0.5000000000000001110 ) ;
#5523 = FACE_BOUND ( 'NONE', #11626, .T. ) ;
#5524 = EDGE_CURVE ( 'NONE', #4850, #2407, #14688, .T. ) ;
#5525 = CARTESIAN_POINT ( 'NONE',  ( -221.5359850654323282, 150.3227202646742455, -2.975602802620230580 ) ) ;
#5526 = ORIENTED_EDGE ( 'NONE', *, *, #6341, .F. ) ;
#5527 = FACE_OUTER_BOUND ( 'NONE', #6210, .T. ) ;
#5528 = VERTEX_POINT ( 'NONE', #1324 ) ;
#5529 = DIRECTION ( 'NONE',  ( 1.000000000000000000, 0.000000000000000000, 0.000000000000000000 ) ) ;
#5530 = DIRECTION ( 'NONE',  ( 1.000000000000000000, 1.669238443041287429E-16, 0.000000000000000000 ) ) ;
#5531 = PLANE ( 'NONE',  #12160 ) ;
#5532 = DIRECTION ( 'NONE',  ( 0.000000000000000000, 0.000000000000000000, -1.000000000000000000 ) ) ;
#5533 = DIRECTION ( 'NONE',  ( 0.000000000000000000, -0.5000000000000019984, -0.8660254037844375974 ) ) ;
#5534 = VECTOR ( 'NONE', #13416, 1000.000000000000000 ) ;
#5535 = CIRCLE ( 'NONE', #7558, 1.000000000000000888 ) ;
#5536 = CARTESIAN_POINT ( 'NONE',  ( 171.7208925888976978, 62.57671370024034729, -0.9107274384406883749 ) ) ;
#5538 = VERTEX_POINT ( 'NONE', #284 ) ;
#5537 = ADVANCED_FACE ( 'NONE', ( #10817 ), #12068, .F. ) ;
#5539 = ORIENTED_EDGE ( 'NONE', *, *, #11357, .T. ) ;
#5540 = CIRCLE ( 'NONE', #460, 1.500000000000001332 ) ;
#5541 = CARTESIAN_POINT ( 'NONE',  ( 201.6516474359912934, 52.64960446646696113, -8.385050746608255778 ) ) ;
#5542 = ORIENTED_EDGE ( 'NONE', *, *, #2996, .F. ) ;
#5543 = DIRECTION ( 'NONE',  ( 0.000000000000000000, 0.000000000000000000, 1.000000000000000000 ) ) ;
#5544 = MANIFOLD_SOLID_BREP ( 'CBORE for M3 Pan Head Screw1[1]', #11667 ) ;
#5545 = CIRCLE ( 'NONE', #7780, 0.5000000000000004441 ) ;
#5546 = DIRECTION ( 'NONE',  ( -0.000000000000000000, 1.000000000000000000, -0.000000000000000000 ) ) ;
#5547 = ORIENTED_EDGE ( 'NONE', *, *, #12429, .F. ) ;
#5548 = ORIENTED_EDGE ( 'NONE', *, *, #7733, .T. ) ;
#5549 = DIRECTION ( 'NONE',  ( -0.000000000000000000, -0.000000000000000000, 1.000000000000000000 ) ) ;
#5550 = ADVANCED_FACE ( 'NONE', ( #9071 ), #9946, .F. ) ;
#5551 = VERTEX_POINT ( 'NONE', #5270 ) ;
#5552 = CARTESIAN_POINT ( 'NONE',  ( 201.2658342953964166, 49.58143373454755931, -3.806719548689701416 ) ) ;
#5553 = DIRECTION ( 'NONE',  ( 0.000000000000000000, -3.469446951953611033E-15, 1.000000000000000000 ) ) ;
#5554 = VECTOR ( 'NONE', #5896, 1000.000000000000114 ) ;
#5555 = CYLINDRICAL_SURFACE ( 'NONE', #994, 0.5000000000000004441 ) ;
#5556 = DIRECTION ( 'NONE',  ( -0.000000000000000000, 1.000000000000000000, 6.938893903907227145E-17 ) ) ;
#5557 = CIRCLE ( 'NONE', #14828, 0.5000000000000004441 ) ;
#5558 = DIRECTION ( 'NONE',  ( 0.000000000000000000, 0.000000000000000000, -1.000000000000000000 ) ) ;
#5559 = AXIS2_PLACEMENT_3D ( 'NONE', #11316, #15010, #4200 ) ;
#5560 = CARTESIAN_POINT ( 'NONE',  ( 122.5806775638430253, 45.00321902537314145, 0.000000000000000000 ) ) ;
#5561 = VECTOR ( 'NONE', #15160, 1000.000000000000000 ) ;
#5562 = ORIENTED_EDGE ( 'NONE', *, *, #859, .T. ) ;
#5563 = CARTESIAN_POINT ( 'NONE',  ( 178.0000000000000853, -179.3058001507315566, -17.19066787724516843 ) ) ;
#5564 = AXIS2_PLACEMENT_3D ( 'NONE', #2952, #12486, #1677 ) ;
#5565 = CARTESIAN_POINT ( 'NONE',  ( -169.9274309510963406, 128.7925441011331031, 1.515441478317341994 ) ) ;
#5566 = CARTESIAN_POINT ( 'NONE',  ( 177.5000000000000853, 17.53993994372674692, -17.50000000000002487 ) ) ;
#5567 = ORIENTED_EDGE ( 'NONE', *, *, #3952, .F. ) ;
#5568 = B_SPLINE_CURVE_WITH_KNOTS ( 'NONE', 3,
 ( #5122, #2439, #12220, #5044 ),
 .UNSPECIFIED., .F., .F.,
 ( 4, 4 ),
 ( 2.380742992386844787E-07, 0.001606744326298692937 ),
 .UNSPECIFIED. ) ;
#5569 = CARTESIAN_POINT ( 'NONE',  ( -217.2107590478593977, 140.9839873040922100, -2.964974570226843742 ) ) ;
#5570 = CARTESIAN_POINT ( 'NONE',  ( 209.6356879938037139, 47.96904352876332922, -5.622739983145865317 ) ) ;
#5571 = ORIENTED_EDGE ( 'NONE', *, *, #12235, .F. ) ;
#5572 = EDGE_CURVE ( 'NONE', #13310, #5662, #8177, .T. ) ;
#5574 = EDGE_CURVE ( 'NONE', #6095, #11949, #356, .T. ) ;
#5573 = EDGE_CURVE ( 'NONE', #6899, #2171, #8995, .T. ) ;
#5575 = LINE ( 'NONE', #2160, #979 ) ;
#5576 = DIRECTION ( 'NONE',  ( 1.000000000000000000, -2.751328491981765035E-32, 3.965082230804130220E-16 ) ) ;
#5577 = CIRCLE ( 'NONE', #14376, 0.5000000000000004441 ) ;
#5578 = CARTESIAN_POINT ( 'NONE',  ( 64.00000000000005684, 64.53993994372673626, 15.00000000000070166 ) ) ;
#5579 = VECTOR ( 'NONE', #8749, 1000.000000000000000 ) ;
#5580 = DIRECTION ( 'NONE',  ( 2.482223822971881035E-17, -2.418222032810046402E-17, 0.9999999999999998890 ) ) ;
#5581 = DIRECTION ( 'NONE',  ( 1.000000000000000000, -0.000000000000000000, -0.000000000000000000 ) ) ;
#5582 = EDGE_LOOP ( 'NONE', ( #11889, #2398, #8375, #14553 ) ) ;
#5583 = FACE_OUTER_BOUND ( 'NONE', #3116, .T. ) ;
#5584 = CARTESIAN_POINT ( 'NONE',  ( -179.8866491758529094, 122.3521977864031243, 9.530069280832647038 ) ) ;
#5585 = DIRECTION ( 'NONE',  ( 0.000000000000000000, 0.000000000000000000, 1.000000000000000000 ) ) ;
#5586 = CARTESIAN_POINT ( 'NONE',  ( 164.0000000000000568, 64.53993994372673626, 15.00000000000000355 ) ) ;
#5587 = ORIENTED_EDGE ( 'NONE', *, *, #2062, .T. ) ;
#5589 = LINE ( 'NONE', #6703, #11121 ) ;
#5588 = VECTOR ( 'NONE', #5929, 1000.000000000000000 ) ;
#5590 = VERTEX_POINT ( 'NONE', #11353 ) ;
#5591 = ORIENTED_EDGE ( 'NONE', *, *, #12594, .F. ) ;
#5592 = STYLED_ITEM ( 'NONE', ( #1022 ), #642 ) ;
#5593 = CARTESIAN_POINT ( 'NONE',  ( 114.0000000000000568, 59.53993994372674337, 13.30000000000035776 ) ) ;
#5594 = DIRECTION ( 'NONE',  ( 0.000000000000000000, 0.000000000000000000, 1.000000000000000000 ) ) ;
#5595 = LINE ( 'NONE', #10405, #2365 ) ;
#5596 = CARTESIAN_POINT ( 'NONE',  ( -173.0522527676590414, 118.1823964801743188, 8.186264704042805818 ) ) ;
#5597 = CARTESIAN_POINT ( 'NONE',  ( -223.0526696604661652, 147.6053417333511106, -2.589170730542551535 ) ) ;
#5598 = CARTESIAN_POINT ( 'NONE',  ( 6.399999999999999467, 0.000000000000000000, 0.000000000000000000 ) ) ;
#5599 = AXIS2_PLACEMENT_3D ( 'NONE', #2358, #11995, #7112 ) ;
#5600 = CARTESIAN_POINT ( 'NONE',  ( -76.50000000000004263, -178.6666270497714777, 53.18093594598651919 ) ) ;
#5601 = VECTOR ( 'NONE', #14729, 1000.000000000000000 ) ;
#5602 = DIRECTION ( 'NONE',  ( 0.000000000000000000, 8.673617379884035472E-17, -1.000000000000000000 ) ) ;
#5603 = EDGE_CURVE ( 'NONE', #12940, #9203, #11692, .T. ) ;
#5604 = CARTESIAN_POINT ( 'NONE',  ( -223.7665658100024189, 146.3262847186648230, -1.606151718348904689 ) ) ;
#5605 = ORIENTED_EDGE ( 'NONE', *, *, #12118, .F. ) ;
#5606 = VERTEX_POINT ( 'NONE', #8918 ) ;
#5607 = DIRECTION ( 'NONE',  ( -0.7900120431063429871, 0.6130913241491365850, 0.000000000000000000 ) ) ;
#5608 = CARTESIAN_POINT ( 'NONE',  ( 190.0000000000000568, -179.8058001507315566, -51.45141194869120937 ) ) ;
#5609 = CIRCLE ( 'NONE', #10390, 0.5000000000000004441 ) ;
#5610 = ORIENTED_EDGE ( 'NONE', *, *, #731, .F. ) ;
#5611 = CARTESIAN_POINT ( 'NONE',  ( -198.5677679834141713, 144.7676449960911498, 2.500000000000000000 ) ) ;
#5612 = FACE_OUTER_BOUND ( 'NONE', #4978, .T. ) ;
#5613 = CARTESIAN_POINT ( 'NONE',  ( 0.000000000000000000, 15.03993994372673804, 38.07518420361041933 ) ) ;
#5614 = ORIENTED_EDGE ( 'NONE', *, *, #1929, .T. ) ;
#5615 = EDGE_CURVE ( 'NONE', #15409, #973, #14807, .T. ) ;
#5616 = VERTEX_POINT ( 'NONE', #598 ) ;
#5617 = CARTESIAN_POINT ( 'NONE',  ( 209.6291075214908801, 33.76515323716659367, -3.385148507280513197 ) ) ;
#5618 = FILL_AREA_STYLE ('',( #10436 ) ) ;
#5619 = ORIENTED_EDGE ( 'NONE', *, *, #3073, .T. ) ;
#5620 = AXIS2_PLACEMENT_3D ( 'NONE', #4338, #12777, #9249 ) ;
#5621 = DIRECTION ( 'NONE',  ( 0.000000000000000000, 1.000000000000000000, 6.938893903907227145E-17 ) ) ;
#5622 = MANIFOLD_SOLID_BREP ( 'Move Face2', #547 ) ;
#5623 = LINE ( 'NONE', #13982, #214 ) ;
#5624 = ORIENTED_EDGE ( 'NONE', *, *, #3843, .F. ) ;
#5625 = ORIENTED_EDGE ( 'NONE', *, *, #921, .F. ) ;
#5626 = DIRECTION ( 'NONE',  ( -0.000000000000000000, -0.000000000000000000, 1.000000000000000000 ) ) ;
#5627 = CARTESIAN_POINT ( 'NONE',  ( 171.7208925888976978, 62.57671370024034729, -0.9107274384406881529 ) ) ;
#5628 = ORIENTED_EDGE ( 'NONE', *, *, #15451, .F. ) ;
#5629 = DIRECTION ( 'NONE',  ( -0.8731965799097679559, 0.4873681696970824095, 0.000000000000000000 ) ) ;
#5630 = CYLINDRICAL_SURFACE ( 'NONE', #9086, 0.5000000000000004441 ) ;
#5631 = FACE_OUTER_BOUND ( 'NONE', #7536, .T. ) ;
#5632 = AXIS2_PLACEMENT_3D ( 'NONE', #13787, #2985, #6471 ) ;
#5633 = CARTESIAN_POINT ( 'NONE',  ( 184.0000000000000568, 17.53993994372673626, 45.99999999999998579 ) ) ;
#5634 = CIRCLE ( 'NONE', #13439, 1.000000000000000888 ) ;
#5635 = PRODUCT ( 'Upper Moving Shear Blade Bar', 'Upper Moving Shear Blade Bar', '', ( #10200 ) ) ;
#5636 = ADVANCED_FACE ( 'NONE', ( #14738 ), #12523, .F. ) ;
#5637 = ORIENTED_EDGE ( 'NONE', *, *, #10664, .T. ) ;
#5638 = CARTESIAN_POINT ( 'NONE',  ( -76.50000000000001421, 15.03993994372673981, -3.075184203610571654 ) ) ;
#5639 = CARTESIAN_POINT ( 'NONE',  ( -174.9627087613145306, 131.1742099673107305, -0.4568654681747568169 ) ) ;
#5640 = CARTESIAN_POINT ( 'NONE',  ( 200.1062858801516597, 40.86394065090267702, 5.000000000000000000 ) ) ;
#5641 = ORIENTED_EDGE ( 'NONE', *, *, #13799, .T. ) ;
#5642 = CARTESIAN_POINT ( 'NONE',  ( -203.7063805325860812, 135.3711971156951677, -4.642206099735014746 ) ) ;
#5643 = CARTESIAN_POINT ( 'NONE',  ( 192.9601959511087728, 50.37386974367067438, -4.870874480120333416 ) ) ;
#5644 = VECTOR ( 'NONE', #14793, 1000.000000000000000 ) ;
#5645 = ORIENTED_EDGE ( 'NONE', *, *, #11620, .T. ) ;
#5646 = CIRCLE ( 'NONE', #7173, 3.499999999999999556 ) ;
#5647 = PLANE ( 'NONE',  #7820 ) ;
#5648 = DIRECTION ( 'NONE',  ( -0.000000000000000000, -0.000000000000000000, 1.000000000000000000 ) ) ;
#5649 = APPLICATION_CONTEXT ( 'automotive_design' ) ;
#5650 = EDGE_CURVE ( 'NONE', #9401, #9986, #4002, .T. ) ;
#5651 = DIRECTION ( 'NONE',  ( -0.000000000000000000, 1.000000000000000000, -0.000000000000000000 ) ) ;
#5652 = EDGE_LOOP ( 'NONE', ( #4581, #7047, #1555, #7393 ) ) ;
#5653 = LINE ( 'NONE', #658, #8397 ) ;
#5654 = EDGE_CURVE ( 'NONE', #10742, #627, #1560, .T. ) ;
#5655 = VERTEX_POINT ( 'NONE', #13631 ) ;
#5656 = CARTESIAN_POINT ( 'NONE',  ( 195.1062858801516597, 40.86394065090267702, 0.000000000000000000 ) ) ;
#5657 = CIRCLE ( 'NONE', #1329, 0.5000000000000001110 ) ;
#5658 = CARTESIAN_POINT ( 'NONE',  ( -178.4568510201948186, 124.9139056227158733, 10.12588066961104261 ) ) ;
#5659 = DIRECTION ( 'NONE',  ( 1.000000000000000000, -1.942890293094024892E-14, 0.000000000000000000 ) ) ;
#5660 = ADVANCED_FACE ( 'NONE', ( #3212, #4630, #5820, #9459, #9154, #9226, #10638 ), #8214, .T. ) ;
#5661 = FACE_OUTER_BOUND ( 'NONE', #8705, .T. ) ;
#5662 = VERTEX_POINT ( 'NONE', #12758 ) ;
#5663 = DIRECTION ( 'NONE',  ( 0.8731965799097684000, -0.4873681696970815769, -0.000000000000000000 ) ) ;
#5664 = VERTEX_POINT ( 'NONE', #14023 ) ;
#5665 = EDGE_LOOP ( 'NONE', ( #12551, #11141, #6260, #14386 ) ) ;
#5666 = CARTESIAN_POINT ( 'NONE',  ( -35.99999999999995026, 64.51493994372674479, 18.50000000000140332 ) ) ;
#5667 = LINE ( 'NONE', #2986, #12297 ) ;
#5668 = VECTOR ( 'NONE', #10045, 1000.000000000000000 ) ;
#5669 = DIRECTION ( 'NONE',  ( 0.000000000000000000, -0.5000000000000006661, 0.8660254037844382635 ) ) ;
#5670 = CARTESIAN_POINT ( 'NONE',  ( -167.8411187277642114, 127.5189611227023363, 3.660767585630689602 ) ) ;
#5671 = CARTESIAN_POINT ( 'NONE',  ( -219.7323164117629801, 149.4657087312641863, -4.974268084325299100 ) ) ;
#5672 = CARTESIAN_POINT ( 'NONE',  ( -111.2071507613730290, 58.10263819636593041, 10.00000000000000178 ) ) ;
#5673 = EDGE_CURVE ( 'NONE', #4933, #12236, #12430, .T. ) ;
#5674 = EDGE_CURVE ( 'NONE', #6130, #11085, #7012, .T. ) ;
#5675 = DIRECTION ( 'NONE',  ( 0.000000000000000000, 0.000000000000000000, 1.000000000000000000 ) ) ;
#5676 = CARTESIAN_POINT ( 'NONE',  ( 17.41029453487719181, 40.04259805664093363, 5.000000000000000000 ) ) ;
#5677 = CARTESIAN_POINT ( 'NONE',  ( -76.50000000000001421, 16.03993994372673981, -3.075184203610571654 ) ) ;
#5678 = CARTESIAN_POINT ( 'NONE',  ( 73.76535645333923696, 38.79159067395544014, 7.600000000000002309 ) ) ;
#5679 = CARTESIAN_POINT ( 'NONE',  ( 178.0000000000000853, 16.03993994372673981, 10.05257423913146475 ) ) ;
#5680 = ORIENTED_EDGE ( 'NONE', *, *, #245, .F. ) ;
#5681 = DIRECTION ( 'NONE',  ( 1.000000000000000000, 0.000000000000000000, 0.000000000000000000 ) ) ;
#5682 = ORIENTED_EDGE ( 'NONE', *, *, #12839, .F. ) ;
#5683 = CARTESIAN_POINT ( 'NONE',  ( 3.011202127489036917E-15, -7.124194613927635977, -3.660532965668818584 ) ) ;
#5684 = LINE ( 'NONE', #15287, #7624 ) ;
#5685 = ORIENTED_EDGE ( 'NONE', *, *, #1988, .T. ) ;
#5686 = CARTESIAN_POINT ( 'NONE',  ( 203.8258924691278082, 51.74121150033466421, -0.9185252821640312870 ) ) ;
#5687 = LINE ( 'NONE', #10268, #8115 ) ;
#5688 = ADVANCED_FACE ( 'NONE', ( #4468 ), #6862, .F. ) ;
#5689 = VECTOR ( 'NONE', #13268, 1000.000000000000000 ) ;
#5690 = CARTESIAN_POINT ( 'NONE',  ( 5.196152422706632024, 9.000000000000003553, 5.000000000000000000 ) ) ;
#5691 = VERTEX_POINT ( 'NONE', #9381 ) ;
#5692 = ORIENTED_EDGE ( 'NONE', *, *, #657, .T. ) ;
#5693 = CARTESIAN_POINT ( 'NONE',  ( 211.8663679066739007, 39.14335912920272875, 0.001962313962203070510 ) ) ;
#5694 =( NAMED_UNIT ( * ) SI_UNIT ( $, .STERADIAN. ) SOLID_ANGLE_UNIT ( ) );
#5695 = EDGE_LOOP ( 'NONE', ( #4498, #6502, #11540, #5390 ) ) ;
#5696 = CARTESIAN_POINT ( 'NONE',  ( 178.0000000000000853, 16.03993994372673981, -3.075184203610571654 ) ) ;
#5697 = VECTOR ( 'NONE', #2463, 1000.000000000000114 ) ;
#5698 = DIRECTION ( 'NONE',  ( 0.000000000000000000, -1.000000000000000000, -4.956352788505162775E-17 ) ) ;
#5699 = CARTESIAN_POINT ( 'NONE',  ( -225.6574687014862661, 142.9384353668704364, 3.546568788011186690 ) ) ;
#5700 = ORIENTED_EDGE ( 'NONE', *, *, #1753, .F. ) ;
#5701 = ORIENTED_EDGE ( 'NONE', *, *, #1234, .T. ) ;
#5702 = CARTESIAN_POINT ( 'NONE',  ( -85.99999999999994316, 59.53993994372674337, 16.70000000000174012 ) ) ;
#5703 = AXIS2_PLACEMENT_3D ( 'NONE', #3048, #1849, #2087 ) ;
#5704 = DIRECTION ( 'NONE',  ( 1.000000000000000000, 0.000000000000000000, 0.000000000000000000 ) ) ;
#5705 = ORIENTED_EDGE ( 'NONE', *, *, #15207, .T. ) ;
#5706 = CARTESIAN_POINT ( 'NONE',  ( -160.1026119161506358, 114.7098309688581708, 2.431557144026069928 ) ) ;
#5707 = EDGE_CURVE ( 'NONE', #11511, #14374, #990, .T. ) ;
#5708 = DIRECTION ( 'NONE',  ( 0.000000000000000000, 0.000000000000000000, -1.000000000000000000 ) ) ;
#5709 = CARTESIAN_POINT ( 'NONE',  ( 200.1062858801516597, 40.86394065090267702, 5.000000000000000000 ) ) ;
#5710 = CIRCLE ( 'NONE', #140, 0.5000000000000004441 ) ;
#5711 = AXIS2_PLACEMENT_3D ( 'NONE', #13301, #1076, #14412 ) ;
#5712 = FACE_OUTER_BOUND ( 'NONE', #11993, .T. ) ;
#5713 = DIRECTION ( 'NONE',  ( 0.4873681696970831312, 0.8731965799097676229, 0.000000000000000000 ) ) ;
#5714 = DIRECTION ( 'NONE',  ( 0.000000000000000000, 1.000000000000000000, 0.000000000000000000 ) ) ;
#5715 = ADVANCED_FACE ( 'NONE', ( #14098 ), #15431, .T. ) ;
#5716 = DIRECTION ( 'NONE',  ( 1.000000000000000000, -2.751328491981765035E-32, 3.965082230804130220E-16 ) ) ;
#5717 = ORIENTED_EDGE ( 'NONE', *, *, #2728, .F. ) ;
#5718 = CARTESIAN_POINT ( 'NONE',  ( -200.1353104204616500, 130.1171604195963880, -2.964974570226841522 ) ) ;
#5719 = CARTESIAN_POINT ( 'NONE',  ( 209.6240687314160880, 33.75364762868482416, -9.385773361654676350 ) ) ;
#5720 = VERTEX_POINT ( 'NONE', #15123 ) ;
#5721 = VECTOR ( 'NONE', #11998, 1000.000000000000000 ) ;
#5722 = CARTESIAN_POINT ( 'NONE',  ( 0.1708300674639772754, 3.045886356309201126, 0.2243700767916273764 ) ) ;
#5723 = DIRECTION ( 'NONE',  ( 0.000000000000000000, 1.734723475976805517E-15, 1.000000000000000000 ) ) ;
#5724 = CARTESIAN_POINT ( 'NONE',  ( -132.4907271922243694, 117.2156449176087847, 5.000000000000000000 ) ) ;
#5725 = ORIENTED_EDGE ( 'NONE', *, *, #518, .F. ) ;
#5726 = EDGE_CURVE ( 'NONE', #14924, #15074, #5138, .T. ) ;
#5727 =( LENGTH_UNIT ( ) NAMED_UNIT ( * ) SI_UNIT ( .MILLI., .METRE. ) );
#5728 = LINE ( 'NONE', #10541, #4088 ) ;
#5729 = CARTESIAN_POINT ( 'NONE',  ( 198.9393012728169765, 49.56711568108339350, -5.111368784863990378 ) ) ;
#5730 = AXIS2_PLACEMENT_3D ( 'NONE', #14892, #14739, #12453 ) ;
#5731 = ORIENTED_EDGE ( 'NONE', *, *, #1967, .F. ) ;
#5732 = DIRECTION ( 'NONE',  ( -1.000000000000000000, 0.000000000000000000, 0.000000000000000000 ) ) ;
#5733 = CARTESIAN_POINT ( 'NONE',  ( -202.2835283783994953, 137.9722283379741725, 10.16010209732750624 ) ) ;
#5734 = PLANE ( 'NONE',  #13325 ) ;
#5735 = CARTESIAN_POINT ( 'NONE',  ( -76.00000000000001421, -178.8058001507315566, 52.19066787724494816 ) ) ;
#5736 = CARTESIAN_POINT ( 'NONE',  ( 172.5293059057019889, 61.25683321636181233, 5.000000000000000000 ) ) ;
#5737 = ORIENTED_EDGE ( 'NONE', *, *, #14334, .F. ) ;
#5738 = ORIENTED_EDGE ( 'NONE', *, *, #8613, .F. ) ;
#5739 = CARTESIAN_POINT ( 'NONE',  ( -152.3841743999474829, 107.5262214188251164, 9.499964102291382773 ) ) ;
#5740 = FACE_BOUND ( 'NONE', #14156, .T. ) ;
#5741 = EDGE_CURVE ( 'NONE', #11585, #13022, #11945, .T. ) ;
#5742 = CARTESIAN_POINT ( 'NONE',  ( 0.000000000000000000, 0.000000000000000000, 0.000000000000000000 ) ) ;
#5743 = CARTESIAN_POINT ( 'NONE',  ( -167.8000917210836747, 127.5924674453244592, 2.732326210438932979 ) ) ;
#5744 = CARTESIAN_POINT ( 'NONE',  ( -223.5878110270859906, 146.6465519720144073, -4.388772443223475150 ) ) ;
#5745 = CIRCLE ( 'NONE', #8031, 3.525000000000002132 ) ;
#5746 = CARTESIAN_POINT ( 'NONE',  ( -216.7216729069047005, 154.8463875879168086, 3.280095325655492111 ) ) ;
#5747 = CARTESIAN_POINT ( 'NONE',  ( 0.2456200930618607225, 1.587713240271468207, -2.750000000000000000 ) ) ;
#5748 = LINE ( 'NONE', #1948, #14215 ) ;
#5749 = CONICAL_SURFACE ( 'NONE', #15062, 4.172000000000013920, 0.7853981633974430610 ) ;
#5750 = DIRECTION ( 'NONE',  ( 3.965082230804130220E-16, 4.956352788505162775E-17, -1.000000000000000000 ) ) ;
#5751 = FACE_OUTER_BOUND ( 'NONE', #9926, .T. ) ;
#5752 = LINE ( 'NONE', #15597, #1057 ) ;
#5753 = ORIENTED_EDGE ( 'NONE', *, *, #7218, .T. ) ;
#5754 = AXIS2_PLACEMENT_3D ( 'NONE', #1933, #13702, #5585 ) ;
#5755 = ORIENTED_EDGE ( 'NONE', *, *, #6228, .T. ) ;
#5756 = DIRECTION ( 'NONE',  ( 0.000000000000000000, 0.000000000000000000, 1.000000000000000000 ) ) ;
#5757 = EDGE_LOOP ( 'NONE', ( #4339, #6154, #6668, #2379 ) ) ;
#5758 = EDGE_CURVE ( 'NONE', #9239, #7288, #1590, .T. ) ;
#5759 = LINE ( 'NONE', #6957, #2605 ) ;
#5760 = DIRECTION ( 'NONE',  ( 1.000000000000000000, 0.000000000000000000, 0.000000000000000000 ) ) ;
#5761 = EDGE_CURVE ( 'NONE', #138, #6739, #3452, .T. ) ;
#5762 = VECTOR ( 'NONE', #4188, 1000.000000000000000 ) ;
#5763 = EDGE_LOOP ( 'NONE', ( #10608, #8550, #8030, #9795, #10279 ) ) ;
#5764 = CIRCLE ( 'NONE', #11067, 1.000000000000000444 ) ;
#5765 = EDGE_LOOP ( 'NONE', ( #3870, #14905, #11264, #9822 ) ) ;
#5766 = CARTESIAN_POINT ( 'NONE',  ( 0.000000000000000000, 0.000000000000000000, 8.000000000000007105 ) ) ;
#5767 = ORIENTED_EDGE ( 'NONE', *, *, #3700, .F. ) ;
#5768 = CARTESIAN_POINT ( 'NONE',  ( 190.0000000000000568, -178.8753867012115961, -29.82329228561640022 ) ) ;
#5769 = CARTESIAN_POINT ( 'NONE',  ( -35.99999999999995026, 64.53993994372673626, 16.70000000000140261 ) ) ;
#5770 = DIRECTION ( 'NONE',  ( -0.000000000000000000, 0.9902680687415702510, -0.1391731009600660485 ) ) ;
#5771 = ORIENTED_EDGE ( 'NONE', *, *, #2728, .T. ) ;
#5772 = VECTOR ( 'NONE', #11525, 1000.000000000000000 ) ;
#5773 = VERTEX_POINT ( 'NONE', #10484 ) ;
#5774 = DIRECTION ( 'NONE',  ( 0.000000000000000000, -1.000000000000000000, -6.938893903907227145E-17 ) ) ;
#5775 = DIRECTION ( 'NONE',  ( 0.000000000000000000, -1.000000000000000000, 0.000000000000000000 ) ) ;
#5776 = CIRCLE ( 'NONE', #7812, 3.525000000000002132 ) ;
#5777 = VERTEX_POINT ( 'NONE', #15274 ) ;
#5778 = CARTESIAN_POINT ( 'NONE',  ( -35.99999999999995026, 64.51493994372674479, 15.00000000000139977 ) ) ;
#5779 = FACE_OUTER_BOUND ( 'NONE', #3873, .T. ) ;
#5780 = CIRCLE ( 'NONE', #6806, 8.000000000000028422 ) ;
#5781 = AXIS2_PLACEMENT_3D ( 'NONE', #14132, #12711, #2056 ) ;
#5782 = EDGE_LOOP ( 'NONE', ( #5680, #7233, #14621, #31 ) ) ;
#5783 = DIRECTION ( 'NONE',  ( -5.518327896226364679E-17, -0.9902680687415713612, 0.1391731009600582492 ) ) ;
#5784 = VERTEX_POINT ( 'NONE', #11901 ) ;
#5785 = FACE_OUTER_BOUND ( 'NONE', #14833, .T. ) ;
#5786 = ADVANCED_FACE ( 'NONE', ( #8135 ), #1075, .F. ) ;
#5787 = CYLINDRICAL_SURFACE ( 'NONE', #484, 0.5000000000000004441 ) ;
#5788 = DIRECTION ( 'NONE',  ( 0.000000000000000000, -0.9902680687415713612, 0.1391731009600582492 ) ) ;
#5789 = CIRCLE ( 'NONE', #219, 1.499999999999994227 ) ;
#5790 = EDGE_LOOP ( 'NONE', ( #9951, #1283 ) ) ;
#5791 = CARTESIAN_POINT ( 'NONE',  ( -189.5834090937817109, 129.2672479736120010, -4.642206099735012970 ) ) ;
#5792 = UNCERTAINTY_MEASURE_WITH_UNIT (LENGTH_MEASURE( 1.000000000000000082E-05 ), #5834, 'distance_accuracy_value', 'NONE');
#5793 = CARTESIAN_POINT ( 'NONE',  ( 191.3780708436489704, 41.94285887643944477, -4.625461852610818880 ) ) ;
#5794 = PRESENTATION_LAYER_ASSIGNMENT (  '', '', ( #3030 ) ) ;
#5795 = ORIENTED_EDGE ( 'NONE', *, *, #1508, .T. ) ;
#5796 = AXIS2_PLACEMENT_3D ( 'NONE', #15008, #14062, #5708 ) ;
#5797 = AXIS2_PLACEMENT_3D ( 'NONE', #323, #4126, #11398 ) ;
#5798 = DIRECTION ( 'NONE',  ( -1.000000000000000000, 0.000000000000000000, 0.000000000000000000 ) ) ;
#5799 = CARTESIAN_POINT ( 'NONE',  ( -4.651904946320617462E-15, 6.534749472788140778, 4.681481898397007235 ) ) ;
#5800 = CARTESIAN_POINT ( 'NONE',  ( -150.8752166464184370, 106.3895273938615702, -4.543781140870890134 ) ) ;
#5801 = VECTOR ( 'NONE', #15237, 1000.000000000000000 ) ;
#5802 = ORIENTED_EDGE ( 'NONE', *, *, #14988, .F. ) ;
#5803 = CIRCLE ( 'NONE', #14620, 1.699999999999996625 ) ;
#5804 = CARTESIAN_POINT ( 'NONE',  ( -2.934533493133625104, 18.80010230637034496, -0.3999999999999975797 ) ) ;
#5805 = VECTOR ( 'NONE', #1776, 1000.000000000000000 ) ;
#5806 = CARTESIAN_POINT ( 'NONE',  ( 208.8060099514817978, 42.07246638764446089, -7.432400171711813996 ) ) ;
#5807 = ORIENTED_EDGE ( 'NONE', *, *, #11754, .T. ) ;
#5808 = LINE ( 'NONE', #24, #7717 ) ;
#5809 = CARTESIAN_POINT ( 'NONE',  ( -213.9961813491638623, 134.6717504882919911, 3.478895870929492595 ) ) ;
#5810 = DIRECTION ( 'NONE',  ( 0.000000000000000000, -0.1391731009600641333, -0.9902680687415704730 ) ) ;
#5811 = DIRECTION ( 'NONE',  ( -3.965082230804130220E-16, 1.090924371466202084E-47, 1.000000000000000000 ) ) ;
#5812 = CARTESIAN_POINT ( 'NONE',  ( -110.0000000000000426, 59.53993994372674337, 10.00000000000000178 ) ) ;
#5813 = ORIENTED_EDGE ( 'NONE', *, *, #5985, .F. ) ;
#5814 = ORIENTED_EDGE ( 'NONE', *, *, #11312, .F. ) ;
#5815 = AXIS2_PLACEMENT_3D ( 'NONE', #1885, #12701, #14120 ) ;
#5816 = DIRECTION ( 'NONE',  ( 1.000000000000000000, 0.000000000000000000, 0.000000000000000000 ) ) ;
#5817 = DIRECTION ( 'NONE',  ( 0.000000000000000000, -0.000000000000000000, -1.000000000000000000 ) ) ;
#5818 = EDGE_CURVE ( 'NONE', #12823, #7872, #7970, .T. ) ;
#5819 = CIRCLE ( 'NONE', #9352, 1.999999999999991118 ) ;
#5820 = FACE_BOUND ( 'NONE', #4542, .T. ) ;
#5821 = CYLINDRICAL_SURFACE ( 'NONE', #11013, 1.700000000000007061 ) ;
#5822 = CARTESIAN_POINT ( 'NONE',  ( -222.9037195049596676, 147.8722093182038293, -4.873412262819154961 ) ) ;
#5823 = CARTESIAN_POINT ( 'NONE',  ( -220.0428052216640538, 148.9356522631746884, 9.942732236775652765 ) ) ;
#5824 = CARTESIAN_POINT ( 'NONE',  ( -136.1405586187959784, 108.3975249866138597, 0.000000000000000000 ) ) ;
#5825 = UNCERTAINTY_MEASURE_WITH_UNIT (LENGTH_MEASURE( 1.000000000000000082E-05 ), #13653, 'distance_accuracy_value', 'NONE');
#5826 = AXIS2_PLACEMENT_3D ( 'NONE', #3895, #7618, #6431 ) ;
#5827 = DIRECTION ( 'NONE',  ( 0.000000000000000000, -4.956352788505162775E-17, 1.000000000000000000 ) ) ;
#5828 = EDGE_CURVE ( 'NONE', #12024, #6168, #3614, .T. ) ;
#5829 = DIRECTION ( 'NONE',  ( 0.000000000000000000, 0.000000000000000000, 1.000000000000000000 ) ) ;
#5830 = CARTESIAN_POINT ( 'NONE',  ( -76.50000000000001421, -179.3058001507315566, 84.88378295107887084 ) ) ;
#5831 = CIRCLE ( 'NONE', #8899, 3.500000000000003109 ) ;
#5832 = CARTESIAN_POINT ( 'NONE',  ( 177.5000000000000853, -179.8058001507315566, -17.19066787724516843 ) ) ;
#5833 = ORIENTED_EDGE ( 'NONE', *, *, #10682, .T. ) ;
#5834 =( LENGTH_UNIT ( ) NAMED_UNIT ( * ) SI_UNIT ( .MILLI., .METRE. ) );
#5835 = EDGE_LOOP ( 'NONE', ( #10237, #1262, #1707, #15397 ) ) ;
#5836 = DIRECTION ( 'NONE',  ( -0.000000000000000000, 1.000000000000000000, -0.000000000000000000 ) ) ;
#5837 = CARTESIAN_POINT ( 'NONE',  ( 0.000000000000000000, 0.000000000000000000, 8.000000000000028422 ) ) ;
#5838 = ORIENTED_EDGE ( 'NONE', *, *, #14295, .F. ) ;
#5839 = FACE_OUTER_BOUND ( 'NONE', #11199, .T. ) ;
#5840 = CARTESIAN_POINT ( 'NONE',  ( -63.50000000000002842, -178.8058001507315566, -30.31842631998718574 ) ) ;
#5841 = VECTOR ( 'NONE', #7494, 1000.000000000000000 ) ;
#5842 = AXIS2_PLACEMENT_3D ( 'NONE', #3668, #2408, #12114 ) ;
#5844 = VERTEX_POINT ( 'NONE', #3374 ) ;
#5843 = EDGE_CURVE ( 'NONE', #11923, #6265, #5595, .T. ) ;
#5845 = EDGE_LOOP ( 'NONE', ( #5349, #818, #13666, #14377 ) ) ;
#5846 = B_SPLINE_CURVE_WITH_KNOTS ( 'NONE', 3,
 ( #5217, #2935, #3951, #6494, #1733, #14680 ),
 .UNSPECIFIED., .F., .F.,
 ( 4, 2, 4 ),
 ( 2.380731629557702153E-07, 0.002336973833157555101, 0.004673709593152154847 ),
 .UNSPECIFIED. ) ;
#5847 = CARTESIAN_POINT ( 'NONE',  ( 211.8797403387081317, 42.53270508615055689, -3.012218501410035998 ) ) ;
#5848 = PRODUCT_DEFINITION ( 'UNKNOWN', '', #704, #604 ) ;
#5849 = ADVANCED_FACE ( 'NONE', ( #10799 ), #12438, .F. ) ;
#5850 = DIRECTION ( 'NONE',  ( -1.000000000000000000, 0.000000000000000000, 0.000000000000000000 ) ) ;
#5851 = ORIENTED_EDGE ( 'NONE', *, *, #2388, .F. ) ;
#5852 = CARTESIAN_POINT ( 'NONE',  ( -64.00000000000002842, -178.8753867012115961, 64.82329228561619061 ) ) ;
#5853 = AXIS2_PLACEMENT_3D ( 'NONE', #2687, #1724, #6560 ) ;
#5854 = CARTESIAN_POINT ( 'NONE',  ( -224.5811800873044604, 144.8667753680074384, 1.831365460742872209 ) ) ;
#5855 = ORIENTED_EDGE ( 'NONE', *, *, #4899, .T. ) ;
#5856 = EDGE_CURVE ( 'NONE', #8789, #7454, #10697, .T. ) ;
#5857 = ORIENTED_EDGE ( 'NONE', *, *, #9134, .T. ) ;
#5858 = VECTOR ( 'NONE', #14341, 1000.000000000000000 ) ;
#5859 = FACE_OUTER_BOUND ( 'NONE', #8045, .T. ) ;
#5860 = CARTESIAN_POINT ( 'NONE',  ( -110.0000000000000426, 19.53993994372674337, 9.999999999999998224 ) ) ;
#5861 = ORIENTED_EDGE ( 'NONE', *, *, #10392, .T. ) ;
#5862 = CARTESIAN_POINT ( 'NONE',  ( -151.6579988274852724, 106.2951400763832766, 9.199440363476590221 ) ) ;
#5863 = DIRECTION ( 'NONE',  ( -0.000000000000000000, 1.000000000000000000, -0.000000000000000000 ) ) ;
#5864 = DIRECTION ( 'NONE',  ( 0.000000000000000000, 0.5000000000000013323, 0.8660254037844380415 ) ) ;
#5866 = AXIS2_PLACEMENT_3D ( 'NONE', #7656, #7577, #4085 ) ;
#5865 = AXIS2_PLACEMENT_3D ( 'NONE', #9970, #14757, #3953 ) ;
#5867 = VERTEX_POINT ( 'NONE', #7255 ) ;
#5868 = ADVANCED_FACE ( 'NONE', ( #13222 ), #10717, .T. ) ;
#5869 = DIRECTION ( 'NONE',  ( 0.4630766004634062072, 0.8863182623094566503, 0.000000000000000000 ) ) ;
#5870 = EDGE_CURVE ( 'NONE', #2296, #13310, #2346, .T. ) ;
#5871 = DIRECTION ( 'NONE',  ( -0.9951762285753402715, 0.09810338464376280876, -0.000000000000000000 ) ) ;
#5872 = CARTESIAN_POINT ( 'NONE',  ( -198.5677679834141713, 144.7676449960911498, 2.500000000000000000 ) ) ;
#5873 = CARTESIAN_POINT ( 'NONE',  ( -151.4086188282879277, 107.2728346664360259, 5.000000000000000000 ) ) ;
#5874 = VERTEX_POINT ( 'NONE', #2499 ) ;
#5875 = CARTESIAN_POINT ( 'NONE',  ( -198.4137021260360711, 129.4968702780754199, -2.964974570226842410 ) ) ;
#5876 = CARTESIAN_POINT ( 'NONE',  ( 198.9883150731717478, 32.15189384935130334, -6.877829860972676457 ) ) ;
#5877 = ORIENTED_EDGE ( 'NONE', *, *, #7094, .F. ) ;
#5878 = APPLICATION_CONTEXT ( 'automotive_design' ) ;
#5879 = AXIS2_PLACEMENT_3D ( 'NONE', #7842, #11457, #14122 ) ;
#5880 = DIRECTION ( 'NONE',  ( 1.000000000000000000, 2.751328491981765035E-32, -3.965082230804130220E-16 ) ) ;
#5881 = CARTESIAN_POINT ( 'NONE',  ( -127.3091761562077409, 106.2673160437096413, 0.000000000000000000 ) ) ;
#5882 = PLANE ( 'NONE',  #4509 ) ;
#5883 = EDGE_CURVE ( 'NONE', #6990, #5844, #10191, .T. ) ;
#5884 = EDGE_LOOP ( 'NONE', ( #1110, #2395 ) ) ;
#5885 = CARTESIAN_POINT ( 'NONE',  ( 193.1007612367029367, 46.15997280778478995, -6.307360761128419036 ) ) ;
#5886 = EDGE_LOOP ( 'NONE', ( #14459, #12036 ) ) ;
#5887 = DIRECTION ( 'NONE',  ( -1.000000000000000000, 0.000000000000000000, 0.000000000000000000 ) ) ;
#5888 = CIRCLE ( 'NONE', #9419, 8.000000000000028422 ) ;
#5889 = CARTESIAN_POINT ( 'NONE',  ( -178.4228374502453107, 119.2657932277225967, 7.804961498744191317 ) ) ;
#5890 = FACE_BOUND ( 'NONE', #659, .T. ) ;
#5891 = CYLINDRICAL_SURFACE ( 'NONE', #15614, 0.5000000000000004441 ) ;
#5892 = CARTESIAN_POINT ( 'NONE',  ( 207.1167095084715868, 46.15093117762712893, -7.185265714380067337 ) ) ;
#5893 = ORIENTED_EDGE ( 'NONE', *, *, #5574, .F. ) ;
#5894 = ORIENTED_EDGE ( 'NONE', *, *, #8190, .T. ) ;
#5895 = CARTESIAN_POINT ( 'NONE',  ( 21.99999999999999289, 1.493456771560197319E-16, -1.219500000000000028 ) ) ;
#5896 = DIRECTION ( 'NONE',  ( 8.659560562354932858E-17, 0.7071067811865474617, -0.7071067811865474617 ) ) ;
#5897 = DIRECTION ( 'NONE',  ( 0.000000000000000000, -1.000000000000000000, -4.956352788505160310E-17 ) ) ;
#5898 = DIRECTION ( 'NONE',  ( 0.000000000000000000, -0.1391731009600586100, 0.9902680687415712502 ) ) ;
#5899 = EDGE_CURVE ( 'NONE', #927, #11071, #3607, .T. ) ;
#5900 = CARTESIAN_POINT ( 'NONE',  ( -221.2834769382098443, 150.7751282116832670, -2.840239297744243885 ) ) ;
#5901 = VECTOR ( 'NONE', #13304, 1000.000000000000000 ) ;
#5902 = FACE_OUTER_BOUND ( 'NONE', #385, .T. ) ;
#5903 = AXIS2_PLACEMENT_3D ( 'NONE', #1453, #12507, #11331 ) ;
#5904 = CARTESIAN_POINT ( 'NONE',  ( 200.1062858801516597, 40.86394065090267702, -219.0000000000000853 ) ) ;
#5905 = DIRECTION ( 'NONE',  ( 0.000000000000000000, -0.9902680687415702510, -0.1391731009600660485 ) ) ;
#5906 = LINE ( 'NONE', #14490, #10702 ) ;
#5907 = DIRECTION ( 'NONE',  ( -0.000000000000000000, -0.000000000000000000, 1.000000000000000000 ) ) ;
#5908 = LINE ( 'NONE', #2195, #4216 ) ;
#5909 = DIRECTION ( 'NONE',  ( 0.000000000000000000, -1.000000000000000000, 0.000000000000000000 ) ) ;
#5910 = ORIENTED_EDGE ( 'NONE', *, *, #2719, .F. ) ;
#5911 = VERTEX_POINT ( 'NONE', #13300 ) ;
#5912 = LINE ( 'NONE', #4570, #15331 ) ;
#5913 = CARTESIAN_POINT ( 'NONE',  ( 184.0000000000000568, -201.3058001507315566, 77.95141194869098911 ) ) ;
#5914 = DIRECTION ( 'NONE',  ( -0.000000000000000000, -0.000000000000000000, 1.000000000000000000 ) ) ;
#5915 = DIRECTION ( 'NONE',  ( 0.000000000000000000, 0.000000000000000000, 1.000000000000000000 ) ) ;
#5916 = DIRECTION ( 'NONE',  ( 0.000000000000000000, -0.000000000000000000, -1.000000000000000000 ) ) ;
#5917 = CARTESIAN_POINT ( 'NONE',  ( -214.8759442515754188, 153.8597017879883424, 3.478855109513426580 ) ) ;
#5918 = ORIENTED_EDGE ( 'NONE', *, *, #15246, .F. ) ;
#5919 = VECTOR ( 'NONE', #2903, 1000.000000000000000 ) ;
#5920 = ORIENTED_EDGE ( 'NONE', *, *, #11845, .T. ) ;
#5921 = CARTESIAN_POINT ( 'NONE',  ( 191.4177849616493461, 42.04274826850978286, -7.631480755160323426 ) ) ;
#5922 = ORIENTED_EDGE ( 'NONE', *, *, #4004, .T. ) ;
#5923 = DIRECTION ( 'NONE',  ( 1.000000000000000000, 0.000000000000000000, 0.000000000000000000 ) ) ;
#5924 = CARTESIAN_POINT ( 'NONE',  ( -222.6691881216298725, 143.9122218626206688, 7.777047806907320115 ) ) ;
#5925 = ORIENTED_EDGE ( 'NONE', *, *, #13174, .T. ) ;
#5926 = EDGE_LOOP ( 'NONE', ( #8509, #3786, #3498, #221 ) ) ;
#5927 = CARTESIAN_POINT ( 'NONE',  ( -85.99999999999994316, 56.53993994372675047, 15.00000000000174794 ) ) ;
#5928 = EDGE_CURVE ( 'NONE', #256, #11858, #5646, .T. ) ;
#5929 = DIRECTION ( 'NONE',  ( -0.000000000000000000, -0.000000000000000000, 1.000000000000000000 ) ) ;
#5930 = ORIENTED_EDGE ( 'NONE', *, *, #4730, .F. ) ;
#5931 = DIRECTION ( 'NONE',  ( -0.8731965799097684000, 0.4873681696970817989, 0.000000000000000000 ) ) ;
#5932 = DIRECTION ( 'NONE',  ( 0.000000000000000000, 0.000000000000000000, -1.000000000000000000 ) ) ;
#5933 = ADVANCED_FACE ( 'NONE', ( #7178 ), #6216, .F. ) ;
#5934 = DIRECTION ( 'NONE',  ( -0.000000000000000000, -6.938893903907227145E-17, 1.000000000000000000 ) ) ;
#5935 = EDGE_CURVE ( 'NONE', #5777, #1807, #14451, .T. ) ;
#5936 = CIRCLE ( 'NONE', #6200, 0.5000000000000004441 ) ;
#5937 = VERTEX_POINT ( 'NONE', #3680 ) ;
#5938 = PRESENTATION_STYLE_ASSIGNMENT (( #11789 ) ) ;
#5939 = APPLICATION_CONTEXT ( 'automotive_design' ) ;
#5940 = DIRECTION ( 'NONE',  ( -0.9099397267342597129, -0.4147405137080060755, 0.000000000000000000 ) ) ;
#5941 = ORIENTED_EDGE ( 'NONE', *, *, #13549, .F. ) ;
#5942 = AXIS2_PLACEMENT_3D ( 'NONE', #11727, #4139, #8979 ) ;
#5943 = CARTESIAN_POINT ( 'NONE',  ( 0.000000000000000000, -2.381569860407207084, -1.374999999999997113 ) ) ;
#5944 = CARTESIAN_POINT ( 'NONE',  ( -64.00000000000002842, 16.03993994372673981, 7.553451883674125344E-16 ) ) ;
#5945 = DIRECTION ( 'NONE',  ( 1.000000000000000000, 0.000000000000000000, 0.000000000000000000 ) ) ;
#5946 = ORIENTED_EDGE ( 'NONE', *, *, #3398, .F. ) ;
#5947 = VERTEX_POINT ( 'NONE', #8589 ) ;
#5948 = CARTESIAN_POINT ( 'NONE',  ( -201.8614823352862970, 146.6162971164513635, 1.515441477536285220 ) ) ;
#5949 = UNCERTAINTY_MEASURE_WITH_UNIT (LENGTH_MEASURE( 1.000000000000000082E-05 ), #13157, 'distance_accuracy_value', 'NONE');
#5950 = CARTESIAN_POINT ( 'NONE',  ( 192.9390872975532716, 31.37216231216662266, -4.138271986312449080 ) ) ;
#5951 = VERTEX_POINT ( 'NONE', #178 ) ;
#5952 = EDGE_CURVE ( 'NONE', #8751, #10460, #14594, .T. ) ;
#5953 = EDGE_CURVE ( 'NONE', #2480, #2355, #14328, .T. ) ;
#5954 = CARTESIAN_POINT ( 'NONE',  ( -152.4086188282879277, 107.2728346664360402, -4.548387523817075895 ) ) ;
#5955 = CARTESIAN_POINT ( 'NONE',  ( -64.00000000000002842, -179.3058001507315566, -17.19066787724516843 ) ) ;
#5956 = ADVANCED_FACE ( 'NONE', ( #7332 ), #6064, .T. ) ;
#5957 = AXIS2_PLACEMENT_3D ( 'NONE', #1758, #6597, #3108 ) ;
#5958 = LINE ( 'NONE', #13515, #10837 ) ;
#5959 = AXIS2_PLACEMENT_3D ( 'NONE', #7013, #10639, #15432 ) ;
#5960 = ORIENTED_EDGE ( 'NONE', *, *, #13956, .T. ) ;
#5961 = CARTESIAN_POINT ( 'NONE',  ( 200.1062858801499829, 40.86394065090222938, 24.40000000000000213 ) ) ;
#5962 = FILL_AREA_STYLE_COLOUR ( '', #799 ) ;
#5963 = CARTESIAN_POINT ( 'NONE',  ( 193.0950460371283839, 35.57958264137020876, -2.685405722344195389 ) ) ;
#5964 = ORIENTED_EDGE ( 'NONE', *, *, #6017, .T. ) ;
#5965 = CARTESIAN_POINT ( 'NONE',  ( 152.8671246545933400, 7.480744990243093362, -7.157132912367466737 ) ) ;
#5966 = LINE ( 'NONE', #10706, #12228 ) ;
#5967 = CARTESIAN_POINT ( 'NONE',  ( -214.8265656857867327, 135.2606554265309740, 1.515400478619088664 ) ) ;
#5968 = DIRECTION ( 'NONE',  ( -1.000000000000000000, 0.000000000000000000, 0.000000000000000000 ) ) ;
#5969 = CYLINDRICAL_SURFACE ( 'NONE', #12340, 1.000000000000000888 ) ;
#5970 = CARTESIAN_POINT ( 'NONE',  ( -212.8994228580217509, 136.6308034654096559, 7.918248976830621011 ) ) ;
#5971 = CIRCLE ( 'NONE', #14775, 1.699999999999993072 ) ;
#5972 = CARTESIAN_POINT ( 'NONE',  ( 208.8124460758720033, 42.05191026284237665, -4.433604294307299298 ) ) ;
#5973 = EDGE_CURVE ( 'NONE', #720, #13191, #585, .T. ) ;
#5974 = ORIENTED_EDGE ( 'NONE', *, *, #8029, .F. ) ;
#5975 = ORIENTED_EDGE ( 'NONE', *, *, #3442, .F. ) ;
#5976 = DIRECTION ( 'NONE',  ( 0.000000000000000000, 0.000000000000000000, 1.000000000000000000 ) ) ;
#5977 = PLANE ( 'NONE',  #15106 ) ;
#5978 = DIRECTION ( 'NONE',  ( -0.000000000000000000, 1.000000000000000000, -0.000000000000000000 ) ) ;
#5979 = DIRECTION ( 'NONE',  ( 0.000000000000000000, 0.9902680687415713612, -0.1391731009600582492 ) ) ;
#5980 = CARTESIAN_POINT ( 'NONE',  ( -136.1405586187959784, 108.3975249866138597, 0.000000000000000000 ) ) ;
#5981 = CARTESIAN_POINT ( 'NONE',  ( -219.0612485848473057, 150.7318302238501246, 9.479016549696966720 ) ) ;
#5982 = PLANE ( 'NONE',  #3871 ) ;
#5983 = CARTESIAN_POINT ( 'NONE',  ( -76.00000000000001421, 15.03993994372673981, -2.575184203610571654 ) ) ;
#5984 = FACE_OUTER_BOUND ( 'NONE', #14368, .T. ) ;
#5985 = EDGE_CURVE ( 'NONE', #8328, #427, #3886, .T. ) ;
#5986 = CARTESIAN_POINT ( 'NONE',  ( -218.4444600228138711, 155.8616726660956715, 2.500000000270498735 ) ) ;
#5987 = EDGE_CURVE ( 'NONE', #7301, #6998, #2626, .T. ) ;
#5988 = DIRECTION ( 'NONE',  ( 1.000000000000000000, 0.000000000000000000, 0.000000000000000000 ) ) ;
#5989 = DIRECTION ( 'NONE',  ( 1.000000000000000000, 2.751328491981765035E-32, -3.965082230804130220E-16 ) ) ;
#5990 = VERTEX_POINT ( 'NONE', #15587 ) ;
#5991 = EDGE_CURVE ( 'NONE', #652, #12666, #11413, .T. ) ;
#5992 = ORIENTED_EDGE ( 'NONE', *, *, #14994, .F. ) ;
#5993 = DIRECTION ( 'NONE',  ( 0.000000000000000000, 0.000000000000000000, -1.000000000000000000 ) ) ;
#5994 = LINE ( 'NONE', #9629, #6866 ) ;
#5995 = CARTESIAN_POINT ( 'NONE',  ( 0.000000000000000000, 6.928203230275487456, 4.000000000000003553 ) ) ;
#5996 = PRESENTATION_STYLE_ASSIGNMENT (( #1166 ) ) ;
#5997 = FACE_BOUND ( 'NONE', #8865, .T. ) ;
#5998 = CARTESIAN_POINT ( 'NONE',  ( -76.00000000000001421, -179.8058001507315566, -17.50000000000002487 ) ) ;
#5999 = CARTESIAN_POINT ( 'NONE',  ( -167.5053995445195767, 127.4304153265770907, 2.500000001036336350 ) ) ;
#6000 = EDGE_LOOP ( 'NONE', ( #7284, #5380 ) ) ;
#6001 = VECTOR ( 'NONE', #2597, 999.9999999999998863 ) ;
#6002 = AXIS2_PLACEMENT_3D ( 'NONE', #4714, #9309, #13071 ) ;
#6003 = EDGE_LOOP ( 'NONE', ( #12271, #13908 ) ) ;
#6004 = CARTESIAN_POINT ( 'NONE',  ( 205.3436520073863107, 47.91354567463725544, -5.626644267508417840 ) ) ;
#6005 = EDGE_CURVE ( 'NONE', #5048, #4760, #7662, .T. ) ;
#6006 = CARTESIAN_POINT ( 'NONE',  ( 0.06730325657896824021, -1.557442666625485250, 8.000000000000008882 ) ) ;
#6007 = ORIENTED_EDGE ( 'NONE', *, *, #2378, .T. ) ;
#6008 = CARTESIAN_POINT ( 'NONE',  ( -225.1775117427411601, 143.7983535990246651, 6.320880672221801611 ) ) ;
#6009 = ORIENTED_EDGE ( 'NONE', *, *, #3398, .T. ) ;
#6010 = VERTEX_POINT ( 'NONE', #8978 ) ;
#6011 = LINE ( 'NONE', #3562, #6289 ) ;
#6012 = DIRECTION ( 'NONE',  ( -0.000000000000000000, -0.000000000000000000, 1.000000000000000000 ) ) ;
#6013 = EDGE_LOOP ( 'NONE', ( #11794, #3789 ) ) ;
#6014 = AXIS2_PLACEMENT_3D ( 'NONE', #9187, #870, #790 ) ;
#6015 = DIRECTION ( 'NONE',  ( -1.000000000000000000, 0.000000000000000000, 0.000000000000000000 ) ) ;
#6016 = CYLINDRICAL_SURFACE ( 'NONE', #10103, 0.4999999999999996114 ) ;
#6017 = EDGE_CURVE ( 'NONE', #4350, #956, #15462, .T. ) ;
#6018 = CARTESIAN_POINT ( 'NONE',  ( 14.00000000000004086, 56.53993994372675047, 15.00000000000104983 ) ) ;
#6019 = EDGE_CURVE ( 'NONE', #8345, #652, #11702, .T. ) ;
#6020 = ORIENTED_EDGE ( 'NONE', *, *, #59, .F. ) ;
#6021 = VECTOR ( 'NONE', #2298, 1000.000000000000114 ) ;
#6022 = CARTESIAN_POINT ( 'NONE',  ( 5.000000000000000000, 6.123233995736766282E-16, 0.000000000000000000 ) ) ;
#6023 = CIRCLE ( 'NONE', #6921, 3.500000000000003109 ) ;
#6024 = PRODUCT_DEFINITION_FORMATION_WITH_SPECIFIED_SOURCE ( 'ANY', '', #13944, .NOT_KNOWN. ) ;
#6025 = ORIENTED_EDGE ( 'NONE', *, *, #938, .F. ) ;
#6026 = CARTESIAN_POINT ( 'NONE',  ( -85.99999999999994316, 64.53993994372673626, 16.70000000000174012 ) ) ;
#6027 = TOROIDAL_SURFACE ( 'NONE', #4240, 1.000000000000000000, 0.5000000000000000000 ) ;
#6028 = EDGE_CURVE ( 'NONE', #235, #6953, #9052, .T. ) ;
#6029 = DIRECTION ( 'NONE',  ( -0.000000000000000000, 1.000000000000000000, -0.000000000000000000 ) ) ;
#6030 = DIRECTION ( 'NONE',  ( -0.2258817899775119320, -0.9741547192086866813, 0.000000000000000000 ) ) ;
#6031 = EDGE_LOOP ( 'NONE', ( #5628, #5277, #631, #7140 ) ) ;
#6032 = ORIENTED_EDGE ( 'NONE', *, *, #10886, .T. ) ;
#6033 = CARTESIAN_POINT ( 'NONE',  ( -169.4320859569187405, 123.9702250307836238, -4.722862203412457660 ) ) ;
#6034 = CARTESIAN_POINT ( 'NONE',  ( 202.4595012533446550, 32.68412682837883665, -9.685340726858029825 ) ) ;
#6035 = ORIENTED_EDGE ( 'NONE', *, *, #422, .T. ) ;
#6036 = LINE ( 'NONE', #12181, #1741 ) ;
#6037 = CARTESIAN_POINT ( 'NONE',  ( -151.4086188282879277, 107.2728346664360259, 5.000000000000004441 ) ) ;
#6038 = AXIS2_PLACEMENT_3D ( 'NONE', #13591, #14773, #14698 ) ;
#6039 = DIRECTION ( 'NONE',  ( -1.000000000000000000, 0.000000000000000000, 0.000000000000000000 ) ) ;
#6040 = AXIS2_PLACEMENT_3D ( 'NONE', #7453, #13190, #6030 ) ;
#6041 = EDGE_LOOP ( 'NONE', ( #14074, #4908, #13529, #351 ) ) ;
#6042 = CARTESIAN_POINT ( 'NONE',  ( 166.3583383998781358, 57.46267437295986014, 5.000000000000000000 ) ) ;
#6043 = CIRCLE ( 'NONE', #4272, 1.499999999999988232 ) ;
#6044 = CARTESIAN_POINT ( 'NONE',  ( 208.8002188652075972, 39.64064887424692785, -1.560527519332197022 ) ) ;
#6045 = ORIENTED_EDGE ( 'NONE', *, *, #1702, .F. ) ;
#6046 = FACE_OUTER_BOUND ( 'NONE', #4091, .T. ) ;
#6047 = CARTESIAN_POINT ( 'NONE',  ( -76.50000000000004263, -179.3753867012116530, 64.38864891670806401 ) ) ;
#6048 = AXIS2_PLACEMENT_3D ( 'NONE', #13027, #14147, #9500 ) ;
#6049 = EDGE_CURVE ( 'NONE', #6990, #12750, #10155, .T. ) ;
#6050 = CARTESIAN_POINT ( 'NONE',  ( -201.1640730962011219, 128.1953734590158263, 1.515400478619091773 ) ) ;
#6051 = AXIS2_PLACEMENT_3D ( 'NONE', #6746, #6822, #10737 ) ;
#6054 = EDGE_CURVE ( 'NONE', #5655, #9587, #80, .T. ) ;
#6053 = ADVANCED_FACE ( 'NONE', ( #2896 ), #5180, .T. ) ;
#6052 = CARTESIAN_POINT ( 'NONE',  ( -151.4086188282879277, 107.2728346664360259, 84.88378295107887084 ) ) ;
#6055 = VERTEX_POINT ( 'NONE', #14789 ) ;
#6056 = CARTESIAN_POINT ( 'NONE',  ( -200.8348121886614024, 140.6195990399117477, 9.578254705571838556 ) ) ;
#6057 = VECTOR ( 'NONE', #10521, 1000.000000000000000 ) ;
#6058 = CARTESIAN_POINT ( 'NONE',  ( 202.8882743124338504, 32.81631024066724933, -8.087096619718394663 ) ) ;
#6059 = ORIENTED_EDGE ( 'NONE', *, *, #9191, .T. ) ;
#6060 = ORIENTED_EDGE ( 'NONE', *, *, #11252, .F. ) ;
#6061 = EDGE_CURVE ( 'NONE', #158, #935, #6917, .T. ) ;
#6062 = CARTESIAN_POINT ( 'NONE',  ( -214.8263955852045797, 135.2609574206205991, 2.431555724346859737 ) ) ;
#6063 = CARTESIAN_POINT ( 'NONE',  ( 0.08285530295197468531, 1.570896314769965940, -7.999999999999981348 ) ) ;
#6064 = PLANE ( 'NONE',  #7430 ) ;
#6065 = CARTESIAN_POINT ( 'NONE',  ( -85.27455057502459113, 65.19100426474074084, 10.00000000000000178 ) ) ;
#6066 = CARTESIAN_POINT ( 'NONE',  ( -70.00000000000000000, -179.3058001507315566, 76.45141194869098911 ) ) ;
#6067 = VECTOR ( 'NONE', #12999, 1000.000000000000000 ) ;
#6068 = CIRCLE ( 'NONE', #7081, 3.500000000000003109 ) ;
#6069 = CARTESIAN_POINT ( 'NONE',  ( -223.3321795807909211, 142.5930735833125027, 5.590921595890676166 ) ) ;
#6070 = FACE_OUTER_BOUND ( 'NONE', #10551, .T. ) ;
#6071 = CARTESIAN_POINT ( 'NONE',  ( -157.2622295109954962, 109.3968164531734857, 9.188529295497616545 ) ) ;
#6072 = ADVANCED_FACE ( 'NONE', ( #10231 ), #13690, .F. ) ;
#6073 = CARTESIAN_POINT ( 'NONE',  ( 14.00000000000004086, 64.53993994372673626, 13.30000000000105231 ) ) ;
#6074 = DIRECTION ( 'NONE',  ( 3.965082230804130220E-16, -0.000000000000000000, -1.000000000000000000 ) ) ;
#6075 = CIRCLE ( 'NONE', #11864, 3.500000000000004885 ) ;
#6076 = DIRECTION ( 'NONE',  ( 0.000000000000000000, 0.000000000000000000, -1.000000000000000000 ) ) ;
#6077 = VERTEX_POINT ( 'NONE', #7719 ) ;
#6078 = AXIS2_PLACEMENT_3D ( 'NONE', #6892, #14283, #3692 ) ;
#6079 = VERTEX_POINT ( 'NONE', #6530 ) ;
#6080 = CARTESIAN_POINT ( 'NONE',  ( 64.00000000000005684, 64.53993994372673626, 18.50000000000070344 ) ) ;
#6081 = DIRECTION ( 'NONE',  ( 0.000000000000000000, 0.000000000000000000, 1.000000000000000000 ) ) ;
#6082 = EDGE_CURVE ( 'NONE', #5068, #13018, #8935, .T. ) ;
#6083 = SURFACE_STYLE_FILL_AREA ( #7199 ) ;
#6084 = CARTESIAN_POINT ( 'NONE',  ( 190.5000000000000568, -179.8058001507315566, 84.88378295107887084 ) ) ;
#6085 = DIRECTION ( 'NONE',  ( 1.000000000000000000, 0.000000000000000000, 0.000000000000000000 ) ) ;
#6086 = DIRECTION ( 'NONE',  ( 1.000000000000000000, 0.000000000000000000, 0.000000000000000000 ) ) ;
#6087 = CIRCLE ( 'NONE', #246, 1.499999999999994449 ) ;
#6088 = ORIENTED_EDGE ( 'NONE', *, *, #7443, .T. ) ;
#6089 = EDGE_CURVE ( 'NONE', #8626, #6095, #6291, .T. ) ;
#6090 = EDGE_LOOP ( 'NONE', ( #3416, #2700, #3631, #9646 ) ) ;
#6091 = CARTESIAN_POINT ( 'NONE',  ( 193.1446408943811548, 35.52021409135998198, -4.254410606405073736 ) ) ;
#6092 = CARTESIAN_POINT ( 'NONE',  ( -220.1303546989248048, 152.8411277130203700, 6.239059799508164694 ) ) ;
#6093 = ORIENTED_EDGE ( 'NONE', *, *, #12661, .F. ) ;
#6094 = CARTESIAN_POINT ( 'NONE',  ( -222.8166798902130665, 143.6204043892651043, 7.418049566996383959 ) ) ;
#6095 = VERTEX_POINT ( 'NONE', #11260 ) ;
#6096 = DIRECTION ( 'NONE',  ( -0.000000000000000000, 1.000000000000000000, -0.000000000000000000 ) ) ;
#6097 = CARTESIAN_POINT ( 'NONE',  ( 209.6025922774668118, 47.99519474844118605, -4.193309970723227309 ) ) ;
#6098 = AXIS2_PLACEMENT_3D ( 'NONE', #3228, #15217, #4410 ) ;
#6099 = ORIENTED_EDGE ( 'NONE', *, *, #12184, .T. ) ;
#6100 = CARTESIAN_POINT ( 'NONE',  ( 70.26535645333922275, 38.79159067395544014, 10.00000000000000178 ) ) ;
#6101 = FACE_OUTER_BOUND ( 'NONE', #14454, .T. ) ;
#6102 = VECTOR ( 'NONE', #13630, 1000.000000000000000 ) ;
#6103 = CARTESIAN_POINT ( 'NONE',  ( -38.32399788034579302, 48.72489408690345414, 10.00000000000000178 ) ) ;
#6104 = AXIS2_PLACEMENT_3D ( 'NONE', #4380, #2010, #6695 ) ;
#6105 = EDGE_LOOP ( 'NONE', ( #15297, #6890, #12282, #1004 ) ) ;
#6106 = DIRECTION ( 'NONE',  ( -0.000000000000000000, 1.000000000000000000, -0.000000000000000000 ) ) ;
#6107 = CIRCLE ( 'NONE', #13649, 1.499999999999997780 ) ;
#6108 = EDGE_LOOP ( 'NONE', ( #13341, #782, #1902, #5359 ) ) ;
#6109 = DIRECTION ( 'NONE',  ( 1.000000000000000000, 0.000000000000000000, 0.000000000000000000 ) ) ;
#6110 = CARTESIAN_POINT ( 'NONE',  ( -151.6962262675657200, 108.2395187408769033, -4.906715952278851489 ) ) ;
#6111 = ORIENTED_EDGE ( 'NONE', *, *, #13657, .F. ) ;
#6112 = ORIENTED_EDGE ( 'NONE', *, *, #2051, .F. ) ;
#6113 = CARTESIAN_POINT ( 'NONE',  ( -175.7692568323954845, 129.7291524912800185, -2.973479603620230893 ) ) ;
#6114 = CARTESIAN_POINT ( 'NONE',  ( 209.6506722393607731, 33.81364540586627498, -6.382933553887647271 ) ) ;
#6115 = ORIENTED_EDGE ( 'NONE', *, *, #6986, .T. ) ;
#6116 = AXIS2_PLACEMENT_3D ( 'NONE', #8572, #3745, #2483 ) ;
#6117 = FACE_OUTER_BOUND ( 'NONE', #9490, .T. ) ;
#6118 = DIRECTION ( 'NONE',  ( 0.4873681696970831312, 0.8731965799097676229, 0.000000000000000000 ) ) ;
#6119 = DIRECTION ( 'NONE',  ( -0.000000000000000000, 1.000000000000000000, -0.000000000000000000 ) ) ;
#6120 = EDGE_CURVE ( 'NONE', #4381, #13651, #8688, .T. ) ;
#6121 = VERTEX_POINT ( 'NONE', #1773 ) ;
#6122 = CARTESIAN_POINT ( 'NONE',  ( -166.2149879755189659, 118.1214081567377150, 2.431557144026069928 ) ) ;
#6123 = CARTESIAN_POINT ( 'NONE',  ( 208.8276044750562335, 41.97590694738037342, -2.864603354092789100 ) ) ;
#6124 = B_SPLINE_CURVE_WITH_KNOTS ( 'NONE', 3,
 ( #11842, #6797, #853, #15219, #11610, #6880, #5611, #1013, #10660, #10734, #2282, #2125, #4573, #15448, #3394, #773, #9395 ),
 .UNSPECIFIED., .F., .F.,
 ( 4, 2, 2, 2, 2, 2, 3, 4 ),
 ( 0.04000000000000142331, 0.2455027589669699362, 0.3041813370740077405, 0.5308033955276700855, 0.6372805264318512908, 0.8233339832829627003, 1.000000000000000000, 1.159999999999998366 ),
 .UNSPECIFIED. ) ;
#6125 = ORIENTED_EDGE ( 'NONE', *, *, #11584, .T. ) ;
#6126 = DIRECTION ( 'NONE',  ( -0.000000000000000000, -0.000000000000000000, -1.000000000000000000 ) ) ;
#6127 = FACE_OUTER_BOUND ( 'NONE', #1096, .T. ) ;
#6128 = CARTESIAN_POINT ( 'NONE',  ( -173.9416064256852508, 115.8726071073731987, 3.216677072105399660 ) ) ;
#6129 = DIRECTION ( 'NONE',  ( 0.000000000000000000, 1.000000000000000000, 1.156482317317871725E-16 ) ) ;
#6130 = VERTEX_POINT ( 'NONE', #6611 ) ;
#6131 = CARTESIAN_POINT ( 'NONE',  ( -202.2835283783994953, 137.9722283379741725, 10.16010209732750624 ) ) ;
#6132 = AXIS2_PLACEMENT_3D ( 'NONE', #10996, #7056, #3718 ) ;
#6133 = LINE ( 'NONE', #7249, #9363 ) ;
#6134 = VERTEX_POINT ( 'NONE', #579 ) ;
#6135 = ORIENTED_EDGE ( 'NONE', *, *, #9243, .F. ) ;
#6136 = CARTESIAN_POINT ( 'NONE',  ( -220.4645760442968481, 140.7127987834906264, 2.431555724346865510 ) ) ;
#6137 = DIRECTION ( 'NONE',  ( -0.000000000000000000, 1.000000000000000000, -0.000000000000000000 ) ) ;
#6138 = ADVANCED_FACE ( 'NONE', ( #15026, #5103 ), #14719, .F. ) ;
#6139 = CARTESIAN_POINT ( 'NONE',  ( -85.99999999999994316, 64.53993994372673626, 15.00000000000174794 ) ) ;
#6140 = DIRECTION ( 'NONE',  ( -0.000000000000000000, 1.000000000000000000, -0.000000000000000000 ) ) ;
#6141 = CARTESIAN_POINT ( 'NONE',  ( -224.4234439893976969, 145.1493843477977066, 0.4584262417075776752 ) ) ;
#6142 = EDGE_CURVE ( 'NONE', #10019, #8250, #4635, .T. ) ;
#6143 = PRODUCT_DEFINITION ( 'UNKNOWN', '', #5011, #9955 ) ;
#6144 = AXIS2_PLACEMENT_3D ( 'NONE', #13408, #7505, #11052 ) ;
#6145 = DIRECTION ( 'NONE',  ( 1.000000000000000000, 0.000000000000000000, 0.000000000000000000 ) ) ;
#6146 = EDGE_CURVE ( 'NONE', #3552, #6055, #7939, .T. ) ;
#6147 = FACE_OUTER_BOUND ( 'NONE', #6961, .T. ) ;
#6148 = VECTOR ( 'NONE', #11748, 1000.000000000000000 ) ;
#6149 = CARTESIAN_POINT ( 'NONE',  ( 163.9288925978260067, 14.41035391906034491, -6.370175303308201364 ) ) ;
#6150 = DIRECTION ( 'NONE',  ( 1.000000000000000000, 0.000000000000000000, 0.000000000000000000 ) ) ;
#6151 = CARTESIAN_POINT ( 'NONE',  ( 21.71949999999999648, 0.000000000000000000, 0.000000000000000000 ) ) ;
#6152 = ORIENTED_EDGE ( 'NONE', *, *, #7718, .F. ) ;
#6153 =( NAMED_UNIT ( * ) PLANE_ANGLE_UNIT ( ) SI_UNIT ( $, .RADIAN. ) );
#6154 = ORIENTED_EDGE ( 'NONE', *, *, #14542, .F. ) ;
#6155 = CARTESIAN_POINT ( 'NONE',  ( 178.0000000000000853, -178.9449732516916072, -29.32815825124560760 ) ) ;
#6156 = LINE ( 'NONE', #3776, #6608 ) ;
#6157 = AXIS2_PLACEMENT_3D ( 'NONE', #5361, #5280, #6787 ) ;
#6158 = LINE ( 'NONE', #283, #2072 ) ;
#6159 =( NAMED_UNIT ( * ) SI_UNIT ( $, .STERADIAN. ) SOLID_ANGLE_UNIT ( ) );
#6160 = DIRECTION ( 'NONE',  ( 0.000000000000000000, 0.000000000000000000, -1.000000000000000000 ) ) ;
#6161 = CARTESIAN_POINT ( 'NONE',  ( -70.00000000000000000, 17.53993994372673271, 45.99999999999998579 ) ) ;
#6162 = CARTESIAN_POINT ( 'NONE',  ( -187.9175675668324175, 138.8130845598205667, 3.478855109513427468 ) ) ;
#6163 = EDGE_CURVE ( 'NONE', #8651, #5154, #4372, .T. ) ;
#6164 = EDGE_CURVE ( 'NONE', #12750, #15193, #14005, .T. ) ;
#6165 = AXIS2_PLACEMENT_3D ( 'NONE', #12431, #13772, #492 ) ;
#6167 = EDGE_CURVE ( 'NONE', #8073, #8771, #15206, .T. ) ;
#6166 =( REPRESENTATION_RELATIONSHIP ('NONE','NONE', #3298, #3806 ) REPRESENTATION_RELATIONSHIP_WITH_TRANSFORMATION ( #6659 )SHAPE_REPRESENTATION_RELATIONSHIP( ) );
#6168 = VERTEX_POINT ( 'NONE', #10465 ) ;
#6169 = VERTEX_POINT ( 'NONE', #4449 ) ;
#6170 = CONICAL_SURFACE ( 'NONE', #1624, 8.000000000000028422, 1.047197551196600296 ) ;
#6171 = CARTESIAN_POINT ( 'NONE',  ( -223.5769481064250499, 146.6660145995820130, 6.853793408916477148 ) ) ;
#6172 = ORIENTED_EDGE ( 'NONE', *, *, #5524, .F. ) ;
#6173 = VECTOR ( 'NONE', #9784, 1000.000000000000000 ) ;
#6174 = CARTESIAN_POINT ( 'NONE',  ( -223.6441180315265456, 146.5456691348633740, 6.731302149999042861 ) ) ;
#6175 = ORIENTED_EDGE ( 'NONE', *, *, #15398, .F. ) ;
#6176 = LINE ( 'NONE', #139, #11317 ) ;
#6177 = CARTESIAN_POINT ( 'NONE',  ( 209.5860849711743015, 48.02841048703755433, -7.191744956496605390 ) ) ;
#6178 = ADVANCED_FACE ( 'NONE', ( #9132 ), #6918, .T. ) ;
#6179 = ORIENTED_EDGE ( 'NONE', *, *, #714, .F. ) ;
#6180 = CARTESIAN_POINT ( 'NONE',  ( 184.0000000000000568, -179.3058001507315566, 74.95141194869098911 ) ) ;
#6181 = DIRECTION ( 'NONE',  ( -0.000000000000000000, 1.486905836551548832E-16, -1.000000000000000000 ) ) ;
#6182 = AXIS2_PLACEMENT_3D ( 'NONE', #14794, #5258, #5033 ) ;
#6183 = CARTESIAN_POINT ( 'NONE',  ( 164.0000000000000568, 64.53993994372673626, 15.00000000000000355 ) ) ;
#6184 = EDGE_LOOP ( 'NONE', ( #459, #12754, #12544, #10634, #14230, #134, #6628, #4493, #6179, #9902, #13577, #8035, #12192, #8484, #9797, #4098, #8559 ) ) ;
#6185 = ORIENTED_EDGE ( 'NONE', *, *, #245, .T. ) ;
#6186 = DIRECTION ( 'NONE',  ( -0.000000000000000000, 1.000000000000000000, -0.000000000000000000 ) ) ;
#6187 = ORIENTED_EDGE ( 'NONE', *, *, #12587, .T. ) ;
#6188 = CARTESIAN_POINT ( 'NONE',  ( -70.00000000000000000, -181.3058001507315566, -39.95141194869120937 ) ) ;
#6189 = CIRCLE ( 'NONE', #7452, 3.525000000000002132 ) ;
#6190 = EDGE_CURVE ( 'NONE', #1354, #9708, #2928, .T. ) ;
#6191 = CARTESIAN_POINT ( 'NONE',  ( -34.79899788034579444, 48.72489408690345414, 0.000000000000000000 ) ) ;
#6192 = ORIENTED_EDGE ( 'NONE', *, *, #2262, .F. ) ;
#6193 = VERTEX_POINT ( 'NONE', #2086 ) ;
#6194 = CARTESIAN_POINT ( 'NONE',  ( -180.1141531658810777, 134.0357633396332915, -0.4547266291960706530 ) ) ;
#6195 = CARTESIAN_POINT ( 'NONE',  ( 201.3139613293953971, 49.56665511821758230, -6.809528532989353344 ) ) ;
#6196 = ORIENTED_EDGE ( 'NONE', *, *, #14081, .T. ) ;
#6197 = FACE_OUTER_BOUND ( 'NONE', #6875, .T. ) ;
#6198 = PLANE ( 'NONE',  #8723 ) ;
#6199 = DIRECTION ( 'NONE',  ( 0.6130913241491352528, 0.7900120431063439863, -6.390853288715847897E-17 ) ) ;
#6200 = AXIS2_PLACEMENT_3D ( 'NONE', #7527, #12325, #6347 ) ;
#6201 = ORIENTED_EDGE ( 'NONE', *, *, #5573, .F. ) ;
#6202 = VECTOR ( 'NONE', #15253, 1000.000000000000000 ) ;
#6203 = CYLINDRICAL_SURFACE ( 'NONE', #3530, 0.4999999999999996114 ) ;
#6204 = CARTESIAN_POINT ( 'NONE',  ( 192.8103048780560584, 31.45858264101640600, -1.000270116828862133 ) ) ;
#6205 = ORIENTED_EDGE ( 'NONE', *, *, #8793, .F. ) ;
#6206 = DIRECTION ( 'NONE',  ( 1.000000000000000000, 0.000000000000000000, 0.000000000000000000 ) ) ;
#6207 = DIRECTION ( 'NONE',  ( -0.000000000000000000, 1.000000000000000000, -0.000000000000000000 ) ) ;
#6208 = CARTESIAN_POINT ( 'NONE',  ( -192.4489746382803048, 130.7761537121523361, -4.642206099735005864 ) ) ;
#6209 = DIRECTION ( 'NONE',  ( 0.000000000000000000, -0.5000000000000012212, -0.8660254037844379305 ) ) ;
#6210 = EDGE_LOOP ( 'NONE', ( #749, #11082, #4167, #63 ) ) ;
#6211 = CARTESIAN_POINT ( 'NONE',  ( -174.6331699355062028, 120.3494046152724763, 9.441255307061881652 ) ) ;
#6212 = CARTESIAN_POINT ( 'NONE',  ( 207.0737247153217311, 35.51262227952910422, -0.2377773810599485560 ) ) ;
#6213 = VECTOR ( 'NONE', #8240, 1000.000000000000000 ) ;
#6214 = VERTEX_POINT ( 'NONE', #12814 ) ;
#6215 = ORIENTED_EDGE ( 'NONE', *, *, #998, .T. ) ;
#6216 = CYLINDRICAL_SURFACE ( 'NONE', #3379, 0.5000000000000004441 ) ;
#6217 = DIRECTION ( 'NONE',  ( -0.000000000000000000, -0.000000000000000000, 1.000000000000000000 ) ) ;
#6218 = EDGE_CURVE ( 'NONE', #1700, #6193, #12662, .T. ) ;
#6219 = DIRECTION ( 'NONE',  ( 1.000000000000000000, 0.000000000000000000, 0.000000000000000000 ) ) ;
#6220 = DIRECTION ( 'NONE',  ( 1.000000000000000000, 0.000000000000000000, 0.000000000000000000 ) ) ;
#6221 = DIRECTION ( 'NONE',  ( 0.000000000000000000, 0.000000000000000000, 1.000000000000000000 ) ) ;
#6222 = AXIS2_PLACEMENT_3D ( 'NONE', #12051, #14257, #4952 ) ;
#6223 = CARTESIAN_POINT ( 'NONE',  ( -215.8266853215729668, 152.1588074852305112, 7.919662025281898998 ) ) ;
#6224 = FACE_OUTER_BOUND ( 'NONE', #2213, .T. ) ;
#6225 = CARTESIAN_POINT ( 'NONE',  ( -35.99999999999995026, 64.51493994372674479, 15.00000000000139977 ) ) ;
#6226 = ORIENTED_EDGE ( 'NONE', *, *, #4068, .T. ) ;
#6227 = DIRECTION ( 'NONE',  ( 1.000000000000000000, 0.000000000000000000, 0.000000000000000000 ) ) ;
#6228 = EDGE_CURVE ( 'NONE', #10747, #6953, #9281, .T. ) ;
#6229 = VERTEX_POINT ( 'NONE', #4610 ) ;
#6230 = CARTESIAN_POINT ( 'NONE',  ( 177.5000000000000853, 17.53993994372674692, -17.50000000000002487 ) ) ;
#6231 = DIRECTION ( 'NONE',  ( -0.000000000000000000, -0.000000000000000000, 1.000000000000000000 ) ) ;
#6232 = PRESENTATION_STYLE_ASSIGNMENT (( #14271 ) ) ;
#6233 = DIRECTION ( 'NONE',  ( 1.000000000000000000, 0.000000000000000000, 0.000000000000000000 ) ) ;
#6234 = DIRECTION ( 'NONE',  ( -0.000000000000000000, 0.000000000000000000, 1.000000000000000000 ) ) ;
#6235 = DIRECTION ( 'NONE',  ( 0.000000000000000000, 0.000000000000000000, -1.000000000000000000 ) ) ;
#6236 = CARTESIAN_POINT ( 'NONE',  ( -192.1704923257120754, 141.1970532186197431, 2.500000000000000000 ) ) ;
#6237 = ORIENTED_EDGE ( 'NONE', *, *, #10181, .T. ) ;
#6238 = DIRECTION ( 'NONE',  ( 0.000000000000000000, 0.000000000000000000, 1.000000000000000000 ) ) ;
#6239 = CARTESIAN_POINT ( 'NONE',  ( 208.8119396302737130, 39.73295740579614943, -6.128637076002331874 ) ) ;
#6240 = CARTESIAN_POINT ( 'NONE',  ( -221.4549156970492163, 150.4679687638771100, 7.826104580404325439 ) ) ;
#6241 = EDGE_LOOP ( 'NONE', ( #13369, #1197, #10050, #7708 ) ) ;
#6242 = AXIS2_PLACEMENT_3D ( 'NONE', #2028, #4315, #9155 ) ;
#6243 = EDGE_CURVE ( 'NONE', #645, #3648, #3276, .T. ) ;
#6244 = CARTESIAN_POINT ( 'NONE',  ( -224.1075752074748948, 145.7153128536473332, 5.693834061489701170 ) ) ;
#6246 = ADVANCED_FACE ( 'NONE', ( #9437 ), #14158, .T. ) ;
#6245 = ADVANCED_FACE ( 'NONE', ( #6759 ), #5647, .F. ) ;
#6247 = ORIENTED_EDGE ( 'NONE', *, *, #15415, .F. ) ;
#6248 = CARTESIAN_POINT ( 'NONE',  ( -172.6903511823495592, 118.8307999792220642, -4.176935792781210743 ) ) ;
#6249 = CARTESIAN_POINT ( 'NONE',  ( 190.6680756494005209, 33.60499951150965359, -5.687464151445976945 ) ) ;
#6250 = ORIENTED_EDGE ( 'NONE', *, *, #11695, .F. ) ;
#6251 = LINE ( 'NONE', #216, #9414 ) ;
#6252 = DIRECTION ( 'NONE',  ( 0.000000000000000000, 1.000000000000000000, 0.000000000000000000 ) ) ;
#6253 = AXIS2_PLACEMENT_3D ( 'NONE', #14269, #10656, #7111 ) ;
#6254 = CARTESIAN_POINT ( 'NONE',  ( 0.000000000000000000, 0.000000000000000000, 0.000000000000000000 ) ) ;
#6255 = VERTEX_POINT ( 'NONE', #4373 ) ;
#6256 = VECTOR ( 'NONE', #384, 1000.000000000000000 ) ;
#6257 = PRODUCT_CONTEXT ( 'NONE', #14795, 'mechanical' ) ;
#6258 = EDGE_LOOP ( 'NONE', ( #11769, #447 ) ) ;
#6259 = DIRECTION ( 'NONE',  ( 1.000000000000000000, 0.000000000000000000, 0.000000000000000000 ) ) ;
#6260 = ORIENTED_EDGE ( 'NONE', *, *, #14994, .T. ) ;
#6261 = CYLINDRICAL_SURFACE ( 'NONE', #8721, 1.500000000000000444 ) ;
#6262 = AXIS2_PLACEMENT_3D ( 'NONE', #2674, #5119, #7423 ) ;
#6263 = LINE ( 'NONE', #13431, #8599 ) ;
#6264 = CARTESIAN_POINT ( 'NONE',  ( -152.4086188282878993, 107.4001535559411167, -4.592095542101958472 ) ) ;
#6265 = VERTEX_POINT ( 'NONE', #3355 ) ;
#6266 = EDGE_LOOP ( 'NONE', ( #10284, #1450, #1958, #12572, #339 ) ) ;
#6267 = CARTESIAN_POINT ( 'NONE',  ( -213.3556830655219585, 148.0789703896194567, -4.640918829492433950 ) ) ;
#6268 =( GEOMETRIC_REPRESENTATION_CONTEXT ( 3 ) GLOBAL_UNCERTAINTY_ASSIGNED_CONTEXT ( ( #2320 ) ) GLOBAL_UNIT_ASSIGNED_CONTEXT ( ( #15284, #13078, #11913 ) ) REPRESENTATION_CONTEXT ( 'NONE', 'WORKASPACE' ) );
#6269 = CARTESIAN_POINT ( 'NONE',  ( 208.8162124854775357, 42.04914431719598156, -1.433821094984975009 ) ) ;
#6270 = CIRCLE ( 'NONE', #11558, 0.5000000000000004441 ) ;
#6271 = VERTEX_POINT ( 'NONE', #12972 ) ;
#6272 = CARTESIAN_POINT ( 'NONE',  ( -139.4318739252458670, 92.47118091487817537, 5.000000000000000000 ) ) ;
#6273 = CARTESIAN_POINT ( 'NONE',  ( -64.00000000000002842, -179.3058001507315566, -30.31842631998718574 ) ) ;
#6274 = DIRECTION ( 'NONE',  ( 0.000000000000000000, -0.9902680687415714722, 0.1391731009600582769 ) ) ;
#6275 = PRODUCT_DEFINITION_FORMATION_WITH_SPECIFIED_SOURCE ( 'ANY', '', #7916, .NOT_KNOWN. ) ;
#6276 = AXIS2_PLACEMENT_3D ( 'NONE', #5488, #7945, #3975 ) ;
#6277 = EDGE_CURVE ( 'NONE', #15478, #1467, #5575, .T. ) ;
#6278 = FILL_AREA_STYLE ('',( #11246 ) ) ;
#6279 = CARTESIAN_POINT ( 'NONE',  ( 191.4070815280707052, 39.69144961696751039, -1.360995051912267106 ) ) ;
#6280 = VERTEX_POINT ( 'NONE', #6690 ) ;
#6281 = DIRECTION ( 'NONE',  ( -0.000000000000000000, -0.000000000000000000, -1.000000000000000000 ) ) ;
#6282 = CARTESIAN_POINT ( 'NONE',  ( -222.1045353819713455, 144.9552801561289357, -3.848506573863026414 ) ) ;
#6283 = CARTESIAN_POINT ( 'NONE',  ( -173.2784152866543934, 122.7799518889917465, -5.329639836781006501 ) ) ;
#6284 = CARTESIAN_POINT ( 'NONE',  ( -85.99999999999994316, 64.53993994372673626, 18.52500000000175007 ) ) ;
#6285 = CARTESIAN_POINT ( 'NONE',  ( -219.6650276661029011, 145.2909210783078890, 9.577123744044234499 ) ) ;
#6286 = CARTESIAN_POINT ( 'NONE',  ( 194.8483215340629613, 47.90965193911861775, -4.864368187704507740 ) ) ;
#6287 = ORIENTED_EDGE ( 'NONE', *, *, #7823, .T. ) ;
#6288 = VERTEX_POINT ( 'NONE', #654 ) ;
#6289 = VECTOR ( 'NONE', #14519, 999.9999999999998863 ) ;
#6290 = AXIS2_PLACEMENT_3D ( 'NONE', #5389, #13820, #1512 ) ;
#6291 = LINE ( 'NONE', #4138, #13970 ) ;
#6292 = DIRECTION ( 'NONE',  ( -0.1562424607007877608, 0.2866315678550999668, -0.9452145987991775744 ) ) ;
#6293 = CARTESIAN_POINT ( 'NONE',  ( -225.4857480675195802, 143.2460998381742456, -0.09261257463428765324 ) ) ;
#6294 = EDGE_CURVE ( 'NONE', #4760, #2448, #5780, .T. ) ;
#6295 = LINE ( 'NONE', #3918, #5644 ) ;
#6296 = AXIS2_PLACEMENT_3D ( 'NONE', #11961, #6119, #7155 ) ;
#6297 = FACE_OUTER_BOUND ( 'NONE', #2249, .T. ) ;
#6298 =( GEOMETRIC_REPRESENTATION_CONTEXT ( 3 ) GLOBAL_UNCERTAINTY_ASSIGNED_CONTEXT ( ( #2964 ) ) GLOBAL_UNIT_ASSIGNED_CONTEXT ( ( #13235, #7109, #14420 ) ) REPRESENTATION_CONTEXT ( 'NONE', 'WORKASPACE' ) );
#6299 = CARTESIAN_POINT ( 'NONE',  ( -215.0595991585972513, 153.5311831015895052, 5.434754235172610137 ) ) ;
#6300 = DIRECTION ( 'NONE',  ( 0.000000000000000000, 0.000000000000000000, 1.000000000000000000 ) ) ;
#6301 = CARTESIAN_POINT ( 'NONE',  ( 19.11029453487719110, 40.04259805664093363, 0.000000000000000000 ) ) ;
#6302 = ORIENTED_EDGE ( 'NONE', *, *, #14370, .F. ) ;
#6303 = EDGE_CURVE ( 'NONE', #13507, #831, #1488, .T. ) ;
#6304 = CARTESIAN_POINT ( 'NONE',  ( -61.94838851346079167, 15.53993994372673981, 37.49999999999991473 ) ) ;
#6305 = VERTEX_POINT ( 'NONE', #3121 ) ;
#6306 = ORIENTED_EDGE ( 'NONE', *, *, #12820, .T. ) ;
#6307 = AXIS2_PLACEMENT_3D ( 'NONE', #910, #8512, #6939 ) ;
#6308 = CARTESIAN_POINT ( 'NONE',  ( -139.4318739252458670, 92.47118091487817537, 0.000000000000000000 ) ) ;
#6309 = CARTESIAN_POINT ( 'NONE',  ( -63.50000000000002842, 17.53993994372673271, 52.49999999999997868 ) ) ;
#6310 = CARTESIAN_POINT ( 'NONE',  ( 215.1062858801516882, 25.86394065090268057, 13.00000000000000178 ) ) ;
#6311 = AXIS2_PLACEMENT_3D ( 'NONE', #2073, #11717, #4518 ) ;
#6312 = SURFACE_STYLE_FILL_AREA ( #7738 ) ;
#6313 = VECTOR ( 'NONE', #711, 1000.000000000000000 ) ;
#6314 = DIRECTION ( 'NONE',  ( 0.000000000000000000, 0.000000000000000000, 1.000000000000000000 ) ) ;
#6315 = DIRECTION ( 'NONE',  ( -0.000000000000000000, 1.000000000000000000, -0.000000000000000000 ) ) ;
#6316 = CIRCLE ( 'NONE', #6571, 0.5000000000000004441 ) ;
#6317 = CARTESIAN_POINT ( 'NONE',  ( -108.0000000000000568, 59.53993994372674337, 20.00000000000000355 ) ) ;
#6318 = CARTESIAN_POINT ( 'NONE',  ( -180.9926919874575333, 132.4923963613727267, 7.919662025281893669 ) ) ;
#6319 = ORIENTED_EDGE ( 'NONE', *, *, #7953, .F. ) ;
#6320 = ADVANCED_FACE ( 'NONE', ( #12737, #1923, #15178, #3503, #9510, #8494, #13276, #4930, #8341, #6197 ), #12104, .F. ) ;
#6321 = CARTESIAN_POINT ( 'NONE',  ( 170.2911098586863545, 111.9959133412127272, 5.000000000000000000 ) ) ;
#6322 = AXIS2_PLACEMENT_3D ( 'NONE', #6819, #8175, #10519 ) ;
#6323 = VECTOR ( 'NONE', #7092, 1000.000000000000000 ) ;
#6324 = AXIS2_PLACEMENT_3D ( 'NONE', #3916, #5030, #2425 ) ;
#6325 = CARTESIAN_POINT ( 'NONE',  ( 193.1265229109121435, 35.50728864820005981, -5.680987958736793075 ) ) ;
#6326 = DIRECTION ( 'NONE',  ( -0.4873681696970817989, -0.8731965799097684000, 0.000000000000000000 ) ) ;
#6327 = ORIENTED_EDGE ( 'NONE', *, *, #5187, .T. ) ;
#6328 = CARTESIAN_POINT ( 'NONE',  ( -216.7216729069043026, 154.8463875879177181, 3.280095325646671167 ) ) ;
#6329 = VERTEX_POINT ( 'NONE', #5954 ) ;
#6330 = DIRECTION ( 'NONE',  ( 0.000000000000000000, 0.000000000000000000, 1.000000000000000000 ) ) ;
#6331 = CARTESIAN_POINT ( 'NONE',  ( 211.8732981324650382, 39.22040580830856982, -1.567042559649178379 ) ) ;
#6332 = VERTEX_POINT ( 'NONE', #11009 ) ;
#6333 = CYLINDRICAL_SURFACE ( 'NONE', #8911, 0.5000000000000000000 ) ;
#6334 = FACE_OUTER_BOUND ( 'NONE', #7554, .T. ) ;
#6335 = AXIS2_PLACEMENT_3D ( 'NONE', #11765, #14196, #3395 ) ;
#6336 = EDGE_CURVE ( 'NONE', #4169, #5101, #5540, .T. ) ;
#6337 = CIRCLE ( 'NONE', #7856, 1.699999999999991518 ) ;
#6338 = CARTESIAN_POINT ( 'NONE',  ( -63.50000000000002842, 15.17911304468679745, 25.93769382960995884 ) ) ;
#6339 = EDGE_LOOP ( 'NONE', ( #4461, #1487, #2786, #5499 ) ) ;
#6340 = EDGE_CURVE ( 'NONE', #1426, #12939, #6036, .T. ) ;
#6341 = EDGE_CURVE ( 'NONE', #12779, #15030, #10859, .T. ) ;
#6342 = EDGE_LOOP ( 'NONE', ( #3706, #13735 ) ) ;
#6343 = CARTESIAN_POINT ( 'NONE',  ( 2.000000000000000000, 1.587713240271470427, 2.750000000000000888 ) ) ;
#6344 = EDGE_CURVE ( 'NONE', #8637, #14616, #2502, .T. ) ;
#6345 = CARTESIAN_POINT ( 'NONE',  ( 178.0000000000000853, -179.3058001507315566, 52.76585208085545275 ) ) ;
#6346 = VERTEX_POINT ( 'NONE', #1360 ) ;
#6347 = DIRECTION ( 'NONE',  ( 0.000000000000000000, 0.000000000000000000, 1.000000000000000000 ) ) ;
#6348 = CIRCLE ( 'NONE', #15142, 3.500000000000004885 ) ;
#6349 = CARTESIAN_POINT ( 'NONE',  ( -76.50000000000001421, 15.03993994372673981, -3.075184203610571654 ) ) ;
#6350 = ORIENTED_EDGE ( 'NONE', *, *, #4196, .F. ) ;
#6351 = EDGE_LOOP ( 'NONE', ( #9846, #8991 ) ) ;
#6352 = VECTOR ( 'NONE', #8652, 1000.000000000000000 ) ;
#6353 = CARTESIAN_POINT ( 'NONE',  ( 14.00000000000004086, 64.53993994372673626, 16.70000000000104734 ) ) ;
#6354 = CARTESIAN_POINT ( 'NONE',  ( 205.4699394944333051, 33.88363592193200446, -7.930995773285529182 ) ) ;
#6355 = EDGE_LOOP ( 'NONE', ( #9140, #3585 ) ) ;
#6356 = CARTESIAN_POINT ( 'NONE',  ( -76.00000000000001421, 15.03993994372673981, -3.075184203610571654 ) ) ;
#6357 = DIRECTION ( 'NONE',  ( 0.000000000000000000, 0.000000000000000000, -1.000000000000000000 ) ) ;
#6358 = LINE ( 'NONE', #14776, #9848 ) ;
#6359 = EDGE_CURVE ( 'NONE', #3126, #592, #12576, .T. ) ;
#6360 = ADVANCED_FACE ( 'NONE', ( #6117 ), #8564, .T. ) ;
#6361 = VECTOR ( 'NONE', #10030, 1000.000000000000000 ) ;
#6362 = FACE_BOUND ( 'NONE', #3522, .T. ) ;
#6363 = CARTESIAN_POINT ( 'NONE',  ( 211.8731694863154758, 39.16394563883312685, -2.997139605818726515 ) ) ;
#6364 = ORIENTED_EDGE ( 'NONE', *, *, #3825, .F. ) ;
#6365 = PLANE ( 'NONE',  #10373 ) ;
#6366 = CARTESIAN_POINT ( 'NONE',  ( 190.0000000000000853, 21.51947656765315386, 25.04661384777570987 ) ) ;
#6367 = CARTESIAN_POINT ( 'NONE',  ( -198.8906912147545540, 132.4339616203728838, -4.642206099735012970 ) ) ;
#6368 = FACE_OUTER_BOUND ( 'NONE', #11256, .T. ) ;
#6369 = VERTEX_POINT ( 'NONE', #12030 ) ;
#6370 = CARTESIAN_POINT ( 'NONE',  ( -213.7840885461983760, 135.0504928752735339, -0.4555467707853347870 ) ) ;
#6372 = CARTESIAN_POINT ( 'NONE',  ( 193.0950460371283839, 35.57958264137020876, -2.685405722344195389 ) ) ;
#6371 = VECTOR ( 'NONE', #8754, 1000.000000000000114 ) ;
#6373 = ORIENTED_EDGE ( 'NONE', *, *, #2457, .F. ) ;
#6374 = EDGE_LOOP ( 'NONE', ( #3046, #1676, #2884, #4585 ) ) ;
#6375 = CIRCLE ( 'NONE', #4335, 8.000000000000028422 ) ;
#6376 = ADVANCED_FACE ( 'NONE', ( #4853 ), #9671, .F. ) ;
#6377 = EDGE_CURVE ( 'NONE', #14684, #12005, #90, .T. ) ;
#6378 = CARTESIAN_POINT ( 'NONE',  ( 164.0000000000000568, 59.53993994372674337, 15.00000000000000355 ) ) ;
#6379 = DIRECTION ( 'NONE',  ( -0.000000000000000000, -0.000000000000000000, -1.000000000000000000 ) ) ;
#6380 = PLANE ( 'NONE',  #3790 ) ;
#6381 = CARTESIAN_POINT ( 'NONE',  ( 2.000000000000000000, 1.587713240271468207, -2.750000000000000000 ) ) ;
#6383 = COLOUR_RGB ( '', 0.09019608, 0.27058824, 0.51372549) ;
#6382 = VECTOR ( 'NONE', #2458, 1000.000000000000000 ) ;
#6384 = CARTESIAN_POINT ( 'NONE',  ( -211.3030747601025610, 151.8655312830997559, 3.478855109513426580 ) ) ;
#6385 = CARTESIAN_POINT ( 'NONE',  ( -86.97455057502459397, 65.19100426474074084, 5.000000000000000000 ) ) ;
#6386 = CARTESIAN_POINT ( 'NONE',  ( 164.0000000000000568, 59.53993994372674337, 15.00000000000000355 ) ) ;
#6387 = EDGE_LOOP ( 'NONE', ( #12046, #9559, #10907, #10179, #14683 ) ) ;
#6388 = DIRECTION ( 'NONE',  ( 1.000000000000000000, 0.000000000000000000, 0.000000000000000000 ) ) ;
#6389 = ORIENTED_EDGE ( 'NONE', *, *, #7544, .T. ) ;
#6390 = EDGE_CURVE ( 'NONE', #3554, #14309, #13123, .T. ) ;
#6391 = EDGE_LOOP ( 'NONE', ( #9779, #9057 ) ) ;
#6392 = DIRECTION ( 'NONE',  ( 0.000000000000000000, 0.000000000000000000, 1.000000000000000000 ) ) ;
#6393 = LINE ( 'NONE', #9944, #7778 ) ;
#6394 = DIRECTION ( 'NONE',  ( 0.000000000000000000, 0.000000000000000000, 1.000000000000000000 ) ) ;
#6395 = DIRECTION ( 'NONE',  ( -0.000000000000000000, 1.000000000000000000, -0.000000000000000000 ) ) ;
#6396 = DIRECTION ( 'NONE',  ( 0.000000000000000000, 0.000000000000000000, 1.000000000000000000 ) ) ;
#6397 = EDGE_CURVE ( 'NONE', #2142, #326, #3014, .T. ) ;
#6398 = CIRCLE ( 'NONE', #817, 1.700000000000007061 ) ;
#6399 = CARTESIAN_POINT ( 'NONE',  ( -221.0074014867128369, 151.2697607195771639, -4.739390644780034023 ) ) ;
#6400 = CARTESIAN_POINT ( 'NONE',  ( -212.2525635541804547, 150.1126023820536375, 7.919662025281898998 ) ) ;
#6401 = ORIENTED_EDGE ( 'NONE', *, *, #14847, .T. ) ;
#6402 = AXIS2_PLACEMENT_3D ( 'NONE', #2184, #834, #3140 ) ;
#6403 = CARTESIAN_POINT ( 'NONE',  ( 20.91029453487719181, 40.04259805664093363, 7.600000000000002309 ) ) ;
#6404 = CARTESIAN_POINT ( 'NONE',  ( 205.4081958545874613, 47.87064854543508829, -4.057643371672452481 ) ) ;
#6405 = CARTESIAN_POINT ( 'NONE',  ( -223.9498498189288682, 145.9979026459368470, 6.124526283558925144 ) ) ;
#6406 = ORIENTED_EDGE ( 'NONE', *, *, #9109, .T. ) ;
#6407 = AXIS2_PLACEMENT_3D ( 'NONE', #14103, #11755, #7824 ) ;
#6408 = CARTESIAN_POINT ( 'NONE',  ( -219.5220412541523274, 149.8943906618940787, 9.781285959214518044 ) ) ;
#6409 = ORIENTED_EDGE ( 'NONE', *, *, #10977, .F. ) ;
#6410 = DIRECTION ( 'NONE',  ( -1.000000000000000000, 0.000000000000000000, 0.000000000000000000 ) ) ;
#6411 = CARTESIAN_POINT ( 'NONE',  ( 224.0000000000000853, 19.53993994372674337, 24.99999999999999645 ) ) ;
#6413 = VERTEX_POINT ( 'NONE', #7153 ) ;
#6412 = VECTOR ( 'NONE', #10619, 1000.000000000000000 ) ;
#6414 = DIRECTION ( 'NONE',  ( -0.000000000000000000, -0.000000000000000000, 1.000000000000000000 ) ) ;
#6415 = DIRECTION ( 'NONE',  ( 1.000000000000000000, 0.000000000000000000, 0.000000000000000000 ) ) ;
#6416 = DIRECTION ( 'NONE',  ( 0.000000000000000000, -1.000000000000000000, 0.000000000000000000 ) ) ;
#6417 = ORIENTED_EDGE ( 'NONE', *, *, #10292, .F. ) ;
#6418 = ADVANCED_BREP_SHAPE_REPRESENTATION ( '', ( #5544, #11070, #12337 ), #4262 ) ;
#6419 = AXIS2_PLACEMENT_3D ( 'NONE', #15591, #996, #12133 ) ;
#6420 = PRODUCT_CONTEXT ( 'NONE', #4533, 'mechanical' ) ;
#6421 = VERTEX_POINT ( 'NONE', #14623 ) ;
#6422 = MECHANICAL_DESIGN_GEOMETRIC_PRESENTATION_REPRESENTATION (  '', ( #2123 ), #1619 ) ;
#6423 = CARTESIAN_POINT ( 'NONE',  ( 194.0000000000000568, 59.53993994372674337, 10.00000000000000178 ) ) ;
#6424 = CARTESIAN_POINT ( 'NONE',  ( -156.0403575966249434, 111.0024509782357285, 9.825479475539728114 ) ) ;
#6425 = ORIENTED_EDGE ( 'NONE', *, *, #1682, .F. ) ;
#6426 = DIRECTION ( 'NONE',  ( 1.000000000000000000, 0.000000000000000000, 0.000000000000000000 ) ) ;
#6427 = CARTESIAN_POINT ( 'NONE',  ( 190.5000000000000568, 15.53993994372673981, -17.50000000000002487 ) ) ;
#6428 = ORIENTED_EDGE ( 'NONE', *, *, #10975, .T. ) ;
#6429 = EDGE_LOOP ( 'NONE', ( #9400, #6425, #9897, #7688 ) ) ;
#6430 = CARTESIAN_POINT ( 'NONE',  ( -206.0179204244930702, 148.9258921110169638, 2.500000000000000000 ) ) ;
#6431 = DIRECTION ( 'NONE',  ( 0.000000000000000000, 0.000000000000000000, -1.000000000000000000 ) ) ;
#6432 = CIRCLE ( 'NONE', #847, 1.700000000000007061 ) ;
#6433 = EDGE_CURVE ( 'NONE', #13079, #9297, #11959, .T. ) ;
#6434 = ORIENTED_EDGE ( 'NONE', *, *, #11392, .F. ) ;
#6435 = CARTESIAN_POINT ( 'NONE',  ( -110.0000000000000426, 59.53993994372674337, 25.00000000000000000 ) ) ;
#6436 = DIRECTION ( 'NONE',  ( -0.4999999999999999445, 0.8660254037844385966, 0.000000000000000000 ) ) ;
#6437 = CARTESIAN_POINT ( 'NONE',  ( -156.7587144051361179, 109.1946030148509408, -4.358407942927352785 ) ) ;
#6438 = CARTESIAN_POINT ( 'NONE',  ( 177.5000000000000853, 15.03993994372673804, 38.07518420361041933 ) ) ;
#6439 = DIRECTION ( 'NONE',  ( -0.000000000000000000, 0.000000000000000000, 1.000000000000000000 ) ) ;
#6440 = CIRCLE ( 'NONE', #9458, 1.000000000000000888 ) ;
#6441 = DIRECTION ( 'NONE',  ( -0.000000000000000000, 1.000000000000000000, -0.000000000000000000 ) ) ;
#6442 = EDGE_LOOP ( 'NONE', ( #12175, #14003 ) ) ;
#6443 = CARTESIAN_POINT ( 'NONE',  ( 190.5000000000000568, -181.3058001507315566, 84.88378295107885663 ) ) ;
#6444 = DIRECTION ( 'NONE',  ( 5.518327896226365911E-17, -0.9902680687415714722, 0.1391731009600582769 ) ) ;
#6445 = CARTESIAN_POINT ( 'NONE',  ( -194.2672495621651478, 127.5518908598051127, -0.4555467707853320669 ) ) ;
#6446 = DIRECTION ( 'NONE',  ( 1.000000000000000000, 0.000000000000000000, 0.000000000000000000 ) ) ;
#6447 = EDGE_LOOP ( 'NONE', ( #1060, #3190, #10004, #802 ) ) ;
#6448 = CARTESIAN_POINT ( 'NONE',  ( -201.1640730962011219, 128.1953734590158263, 3.478895870929496148 ) ) ;
#6449 = CARTESIAN_POINT ( 'NONE',  ( 207.0901250877858217, 35.54806830018342367, -3.235595374952740855 ) ) ;
#6450 = EDGE_CURVE ( 'NONE', #10552, #3344, #13848, .T. ) ;
#6451 = EDGE_CURVE ( 'NONE', #12140, #5020, #15488, .T. ) ;
#6452 = ORIENTED_EDGE ( 'NONE', *, *, #10204, .T. ) ;
#6453 = EDGE_CURVE ( 'NONE', #5257, #7692, #208, .T. ) ;
#6454 = AXIS2_PLACEMENT_3D ( 'NONE', #3264, #10147, #13996 ) ;
#6455 = DIRECTION ( 'NONE',  ( 0.000000000000000000, -1.000000000000000000, 0.000000000000000000 ) ) ;
#6456 = CARTESIAN_POINT ( 'NONE',  ( -173.4445345933175986, 43.15250799526725700, 5.000000000000000000 ) ) ;
#6457 = CARTESIAN_POINT ( 'NONE',  ( 178.0000000000000853, 16.03993994372673981, 7.553451883674125344E-16 ) ) ;
#6458 = DIRECTION ( 'NONE',  ( -0.000000000000000000, -0.000000000000000000, 1.000000000000000000 ) ) ;
#6459 = ORIENTED_EDGE ( 'NONE', *, *, #13028, .T. ) ;
#6460 = CARTESIAN_POINT ( 'NONE',  ( 0.2456200930618618050, 1.587713240271470427, 2.750000000000000888 ) ) ;
#6461 = EDGE_CURVE ( 'NONE', #720, #14008, #11088, .T. ) ;
#6462 = AXIS2_PLACEMENT_3D ( 'NONE', #1103, #9406, #2214 ) ;
#6463 =( REPRESENTATION_RELATIONSHIP ('NONE','NONE', #3298, #11876 ) REPRESENTATION_RELATIONSHIP_WITH_TRANSFORMATION ( #11924 )SHAPE_REPRESENTATION_RELATIONSHIP( ) );
#6464 = DIRECTION ( 'NONE',  ( 0.000000000000000000, 0.1391731009600592484, 0.9902680687415712502 ) ) ;
#6465 = CARTESIAN_POINT ( 'NONE',  ( 5.799999999999999822, 4.618802153516981868, 8.000000000000007105 ) ) ;
#6466 = ORIENTED_EDGE ( 'NONE', *, *, #2174, .F. ) ;
#6467 = AXIS2_PLACEMENT_3D ( 'NONE', #13039, #892, #5723 ) ;
#6468 = DIRECTION ( 'NONE',  ( -0.000000000000000000, -0.000000000000000000, 1.000000000000000000 ) ) ;
#6469 = EDGE_LOOP ( 'NONE', ( #869, #3477, #6327, #11868 ) ) ;
#6470 = VERTEX_POINT ( 'NONE', #2877 ) ;
#6471 = DIRECTION ( 'NONE',  ( 0.000000000000000000, 0.000000000000000000, 1.000000000000000000 ) ) ;
#6472 = DIRECTION ( 'NONE',  ( 0.000000000000000000, 0.000000000000000000, 1.000000000000000000 ) ) ;
#6473 = DIRECTION ( 'NONE',  ( 0.000000000000000000, -0.4999999999999991118, 0.8660254037844390407 ) ) ;
#6474 = LINE ( 'NONE', #1561, #4455 ) ;
#6475 = CARTESIAN_POINT ( 'NONE',  ( -216.6908943189923207, 154.8992719724514302, 2.316389262299374252 ) ) ;
#6476 = CARTESIAN_POINT ( 'NONE',  ( -194.7616377892423714, 140.1172406977107130, 7.919662025281898998 ) ) ;
#6477 = ORIENTED_EDGE ( 'NONE', *, *, #3272, .F. ) ;
#6478 = AXIS2_PLACEMENT_3D ( 'NONE', #264, #5250, #1696 ) ;
#6479 = ADVANCED_FACE ( 'NONE', ( #4046 ), #11314, .T. ) ;
#6480 = DIRECTION ( 'NONE',  ( 0.000000000000000000, 1.734723475976805517E-15, 1.000000000000000000 ) ) ;
#6481 = EDGE_CURVE ( 'NONE', #5077, #8326, #12826, .T. ) ;
#6482 = PRODUCT_DEFINITION_CONTEXT ( 'detailed design', #9991, 'design' ) ;
#6483 = CARTESIAN_POINT ( 'NONE',  ( 183.0404880503516267, 40.86394065090267702, 0.000000000000000000 ) ) ;
#6484 = ADVANCED_FACE ( 'NONE', ( #12255 ), #9987, .F. ) ;
#6485 = FACE_OUTER_BOUND ( 'NONE', #6469, .T. ) ;
#6486 = CARTESIAN_POINT ( 'NONE',  ( -219.4693564985508942, 154.0254097482049929, 1.294062626359073542 ) ) ;
#6487 = ORIENTED_EDGE ( 'NONE', *, *, #1795, .F. ) ;
#6488 = CARTESIAN_POINT ( 'NONE',  ( -220.8889415488412169, 151.4820002933464025, 7.400835299683578228 ) ) ;
#6489 = ORIENTED_EDGE ( 'NONE', *, *, #3089, .T. ) ;
#6490 = CARTESIAN_POINT ( 'NONE',  ( -169.4759604733452250, 124.5898855086296919, -4.204736276848058729 ) ) ;
#6491 = DIRECTION ( 'NONE',  ( 0.000000000000000000, -0.000000000000000000, -1.000000000000000000 ) ) ;
#6492 = ORIENTED_EDGE ( 'NONE', *, *, #2623, .F. ) ;
#6493 = CARTESIAN_POINT ( 'NONE',  ( 177.5000000000000853, 16.03993994372673981, 24.94742576086838781 ) ) ;
#6494 = CARTESIAN_POINT ( 'NONE',  ( 0.06809871960541388769, 7.710219529346588274, -2.645508037661862932 ) ) ;
#6495 = CARTESIAN_POINT ( 'NONE',  ( 193.3006371371548369, 56.51400776751751920, 0.000000000000000000 ) ) ;
#6496 = VERTEX_POINT ( 'NONE', #14930 ) ;
#6497 = ADVANCED_FACE ( 'NONE', ( #9907 ), #10059, .F. ) ;
#6498 = DIRECTION ( 'NONE',  ( 0.000000000000000000, 0.000000000000000000, 1.000000000000000000 ) ) ;
#6499 = EDGE_LOOP ( 'NONE', ( #349, #4720, #13528, #8243 ) ) ;
#6500 = CARTESIAN_POINT ( 'NONE',  ( -35.99999999999995026, 64.53993994372673626, 18.50000000000140332 ) ) ;
#6501 = CARTESIAN_POINT ( 'NONE',  ( -157.4596430032548540, 110.7948475882922850, 9.623760898223428839 ) ) ;
#6502 = ORIENTED_EDGE ( 'NONE', *, *, #4226, .F. ) ;
#6503 = DIRECTION ( 'NONE',  ( 0.000000000000000000, 0.7071067811865474617, 0.7071067811865474617 ) ) ;
#6504 = CARTESIAN_POINT ( 'NONE',  ( 172.0899380277727744, 70.88000906936352408, -0.9107274384406883749 ) ) ;
#6505 = VERTEX_POINT ( 'NONE', #12488 ) ;
#6506 = ORIENTED_EDGE ( 'NONE', *, *, #8851, .T. ) ;
#6507 = CARTESIAN_POINT ( 'NONE',  ( -192.1704923257120754, 141.1970532186197431, 2.500000000000000000 ) ) ;
#6508 = EDGE_CURVE ( 'NONE', #7789, #15483, #8067, .T. ) ;
#6509 = CARTESIAN_POINT ( 'NONE',  ( 193.1007612367029367, 46.15997280778478995, -6.307360761128419036 ) ) ;
#6510 = ORIENTED_EDGE ( 'NONE', *, *, #681, .T. ) ;
#6511 = CARTESIAN_POINT ( 'NONE',  ( -110.0000000000000426, 19.53993994372674337, 24.99999999999999645 ) ) ;
#6512 = DIRECTION ( 'NONE',  ( -1.000000000000000000, 0.000000000000000000, 0.000000000000000000 ) ) ;
#6513 = AXIS2_PLACEMENT_3D ( 'NONE', #8948, #11229, #4033 ) ;
#6514 = LINE ( 'NONE', #10139, #3258 ) ;
#6515 = CARTESIAN_POINT ( 'NONE',  ( 164.0000000000000568, 59.53993994372674337, 13.29999999999999538 ) ) ;
#6516 = EDGE_CURVE ( 'NONE', #9609, #3320, #1230, .T. ) ;
#6517 = EDGE_CURVE ( 'NONE', #2746, #4804, #9724, .T. ) ;
#6518 = AXIS2_PLACEMENT_3D ( 'NONE', #14889, #8916, #3859 ) ;
#6519 = DIRECTION ( 'NONE',  ( 0.000000000000000000, 0.000000000000000000, -1.000000000000000000 ) ) ;
#6520 = VERTEX_POINT ( 'NONE', #6272 ) ;
#6521 = FACE_OUTER_BOUND ( 'NONE', #7437, .T. ) ;
#6522 = CARTESIAN_POINT ( 'NONE',  ( -220.9124392735551226, 147.2477244607945579, -4.927242291365885762 ) ) ;
#6523 = CIRCLE ( 'NONE', #2724, 338.5619230110239641 ) ;
#6524 = CARTESIAN_POINT ( 'NONE',  ( -181.1480734112017501, 126.1383063644306617, -5.230826428279600648 ) ) ;
#6525 = CARTESIAN_POINT ( 'NONE',  ( -76.50000000000001421, -181.3058001507315566, 84.88378295107885663 ) ) ;
#6526 = EDGE_LOOP ( 'NONE', ( #2016, #15260, #1788, #306 ) ) ;
#6527 = CARTESIAN_POINT ( 'NONE',  ( -191.4964613557999655, 125.7493975051623352, 1.515400478619084224 ) ) ;
#6528 = CARTESIAN_POINT ( 'NONE',  ( 198.8340532681795594, 32.16525826020106393, -3.739820046187162905 ) ) ;
#6529 = ORIENTED_EDGE ( 'NONE', *, *, #6049, .F. ) ;
#6530 = CARTESIAN_POINT ( 'NONE',  ( 177.5000000000000853, 16.03993994372673626, 52.49999999999997868 ) ) ;
#6531 = PRODUCT_DEFINITION_FORMATION_WITH_SPECIFIED_SOURCE ( 'ANY', '', #15450, .NOT_KNOWN. ) ;
#6532 = DIRECTION ( 'NONE',  ( -0.000000000000000000, -0.000000000000000000, 1.000000000000000000 ) ) ;
#6533 = CIRCLE ( 'NONE', #12062, 2.749999999999999112 ) ;
#6534 = CARTESIAN_POINT ( 'NONE',  ( 184.0000000000000568, 17.53993994372673981, -10.99999999999999645 ) ) ;
#6536 = ADVANCED_FACE ( 'NONE', ( #12333 ), #5276, .T. ) ;
#6535 = EDGE_CURVE ( 'NONE', #6993, #13446, #6514, .T. ) ;
#6537 = DIRECTION ( 'NONE',  ( -0.000000000000000000, 1.000000000000000000, -0.000000000000000000 ) ) ;
#6538 = ORIENTED_EDGE ( 'NONE', *, *, #9592, .T. ) ;
#6539 = LINE ( 'NONE', #7564, #15480 ) ;
#6540 = CARTESIAN_POINT ( 'NONE',  ( -219.4661802592007689, 154.0311004795854046, 7.909502539118774322 ) ) ;
#6541 = LINE ( 'NONE', #7887, #14815 ) ;
#6542 = VECTOR ( 'NONE', #1164, 1000.000000000000000 ) ;
#6543 = EDGE_CURVE ( 'NONE', #4287, #6660, #9329, .T. ) ;
#6544 = DIRECTION ( 'NONE',  ( -0.000000000000000000, -0.000000000000000000, 1.000000000000000000 ) ) ;
#6545 = ORIENTED_EDGE ( 'NONE', *, *, #11057, .T. ) ;
#6546 = CARTESIAN_POINT ( 'NONE',  ( -136.1405586187959784, 108.3975249866138597, 0.000000000000000000 ) ) ;
#6547 = AXIS2_PLACEMENT_3D ( 'NONE', #8205, #825, #5659 ) ;
#6548 = EDGE_LOOP ( 'NONE', ( #10917, #13473, #3091, #4371 ) ) ;
#6549 = ORIENTED_EDGE ( 'NONE', *, *, #11530, .T. ) ;
#6550 = CARTESIAN_POINT ( 'NONE',  ( -76.00000000000001421, -179.3058001507315566, -51.45141194869120227 ) ) ;
#6551 = DIRECTION ( 'NONE',  ( -1.000000000000000000, 0.000000000000000000, 0.000000000000000000 ) ) ;
#6552 = B_SPLINE_CURVE_WITH_KNOTS ( 'NONE', 3,
 ( #6877, #11838, #1011, #850, #8229 ),
 .UNSPECIFIED., .F., .F.,
 ( 4, 1, 4 ),
 ( 0.02346780518444461713, 0.02385965792372440192, 0.02425151066300419017 ),
 .UNSPECIFIED. ) ;
#6553 = CARTESIAN_POINT ( 'NONE',  ( 190.2479883433758800, 63.36949047362622167, 5.000000000000000000 ) ) ;
#6554 = CARTESIAN_POINT ( 'NONE',  ( -219.4360840196858646, 154.0850226169894768, 3.058976617618253346 ) ) ;
#6555 = CARTESIAN_POINT ( 'NONE',  ( 177.5000000000000853, 14.97035339324670744, 37.58005016923963382 ) ) ;
#6556 = VERTEX_POINT ( 'NONE', #6596 ) ;
#6557 = AXIS2_PLACEMENT_3D ( 'NONE', #4924, #7228, #12097 ) ;
#6558 = EDGE_CURVE ( 'NONE', #5784, #14668, #11396, .T. ) ;
#6559 = DIRECTION ( 'NONE',  ( 0.000000000000000000, 0.000000000000000000, 1.000000000000000000 ) ) ;
#6560 = DIRECTION ( 'NONE',  ( 0.000000000000000000, 0.000000000000000000, 1.000000000000000000 ) ) ;
#6561 = AXIS2_PLACEMENT_3D ( 'NONE', #10631, #11893, #10709 ) ;
#6562 = CARTESIAN_POINT ( 'NONE',  ( 120.8806775638430224, 45.00321902537314145, 5.000000000000000000 ) ) ;
#6563 = ORIENTED_EDGE ( 'NONE', *, *, #7244, .T. ) ;
#6564 = VECTOR ( 'NONE', #13111, 1000.000000000000000 ) ;
#6565 = ADVANCED_FACE ( 'NONE', ( #321, #5159 ), #5399, .F. ) ;
#6566 = AXIS2_PLACEMENT_3D ( 'NONE', #8960, #12562, #1757 ) ;
#6567 = CARTESIAN_POINT ( 'NONE',  ( -219.6570823573851783, 153.6890694041141217, 4.765787677119769583 ) ) ;
#6568 = VERTEX_POINT ( 'NONE', #13991 ) ;
#6569 = CARTESIAN_POINT ( 'NONE',  ( -170.4088383823848574, 122.9184882974554256, -5.007687358117594911 ) ) ;
#6570 = FACE_OUTER_BOUND ( 'NONE', #10273, .T. ) ;
#6571 = AXIS2_PLACEMENT_3D ( 'NONE', #1605, #12336, #4048 ) ;
#6572 = ORIENTED_EDGE ( 'NONE', *, *, #11020, .F. ) ;
#6573 = DIRECTION ( 'NONE',  ( 0.000000000000000000, 0.000000000000000000, 1.000000000000000000 ) ) ;
#6574 = DIRECTION ( 'NONE',  ( -0.000000000000000000, -0.5000000000000018874, -0.8660254037844375974 ) ) ;
#6575 = EDGE_CURVE ( 'NONE', #12789, #12371, #12584, .T. ) ;
#6576 = CIRCLE ( 'NONE', #15363, 1.499999999999995115 ) ;
#6577 = DIRECTION ( 'NONE',  ( 1.000000000000000000, 0.000000000000000000, 0.000000000000000000 ) ) ;
#6578 = ORIENTED_EDGE ( 'NONE', *, *, #13242, .F. ) ;
#6579 = CIRCLE ( 'NONE', #7080, 1.500000000000001332 ) ;
#6580 = AXIS2_PLACEMENT_3D ( 'NONE', #6457, #2971, #7721 ) ;
#6581 = PRODUCT_CONTEXT ( 'NONE', #2417, 'mechanical' ) ;
#6582 = ORIENTED_EDGE ( 'NONE', *, *, #4444, .F. ) ;
#6583 = CARTESIAN_POINT ( 'NONE',  ( 172.5293059057019889, 61.25683321636181233, 10.00000000000000178 ) ) ;
#6584 = ORIENTED_EDGE ( 'NONE', *, *, #7385, .F. ) ;
#6585 = DIRECTION ( 'NONE',  ( 0.8731965799097686221, -0.4873681696970812438, -0.000000000000000000 ) ) ;
#6586 = FACE_OUTER_BOUND ( 'NONE', #6857, .T. ) ;
#6587 = AXIS2_PLACEMENT_3D ( 'NONE', #13570, #11529, #10347 ) ;
#6588 = ORIENTED_EDGE ( 'NONE', *, *, #6167, .F. ) ;
#6589 = VERTEX_POINT ( 'NONE', #11546 ) ;
#6590 = CARTESIAN_POINT ( 'NONE',  ( -167.5010204568278027, 127.4382611495783237, 1.515441478572621570 ) ) ;
#6591 = CARTESIAN_POINT ( 'NONE',  ( 178.0000000000000853, -178.8058001507315566, 52.19066787724494816 ) ) ;
#6592 = AXIS2_PLACEMENT_3D ( 'NONE', #13705, #8912, #6388 ) ;
#6593 = ORIENTED_EDGE ( 'NONE', *, *, #380, .T. ) ;
#6594 = DIRECTION ( 'NONE',  ( -0.000000000000000000, 1.000000000000000000, 1.156482317317871725E-16 ) ) ;
#6595 = DIRECTION ( 'NONE',  ( 1.000000000000000000, 0.000000000000000000, 0.000000000000000000 ) ) ;
#6596 = CARTESIAN_POINT ( 'NONE',  ( 0.7145311798163258565, -9.237604307034018802, 2.775557561562891351E-14 ) ) ;
#6597 = DIRECTION ( 'NONE',  ( 1.000000000000000000, 0.000000000000000000, 0.000000000000000000 ) ) ;
#6598 = CARTESIAN_POINT ( 'NONE',  ( -64.00000000000002842, -179.8058001507315566, 52.49999999999997868 ) ) ;
#6599 = AXIS2_PLACEMENT_3D ( 'NONE', #3063, #13946, #6773 ) ;
#6600 = DIRECTION ( 'NONE',  ( 0.000000000000000000, -4.956352788505162775E-17, 1.000000000000000000 ) ) ;
#6601 = VERTEX_POINT ( 'NONE', #1909 ) ;
#6602 = FACE_OUTER_BOUND ( 'NONE', #9506, .T. ) ;
#6603 = CARTESIAN_POINT ( 'NONE',  ( -189.8662655649658859, 135.3588663075204579, -4.640918829492423292 ) ) ;
#6604 = ORIENTED_EDGE ( 'NONE', *, *, #9339, .T. ) ;
#6605 = CARTESIAN_POINT ( 'NONE',  ( -214.8265656857867327, 135.2606554265309740, 1.515400478619088664 ) ) ;
#6606 = CARTESIAN_POINT ( 'NONE',  ( 207.2819921120892275, 50.35227183911742088, -8.638656677529437999 ) ) ;
#6607 = VERTEX_POINT ( 'NONE', #1833 ) ;
#6608 = VECTOR ( 'NONE', #5041, 1000.000000000000000 ) ;
#6609 = B_SPLINE_CURVE_WITH_KNOTS ( 'NONE', 3,
 ( #6460, #11115, #11191, #7483 ),
 .UNSPECIFIED., .F., .F.,
 ( 4, 4 ),
 ( 2.380742992386783113E-07, 0.001606744326298686649 ),
 .UNSPECIFIED. ) ;
#6610 = EDGE_CURVE ( 'NONE', #8626, #4614, #9551, .T. ) ;
#6611 = CARTESIAN_POINT ( 'NONE',  ( 2.000000000000000000, 3.175426480542944407, 0.000000000000000000 ) ) ;
#6612 = LINE ( 'NONE', #10466, #6202 ) ;
#6613 = CIRCLE ( 'NONE', #7616, 0.5000000000000004441 ) ;
#6614 = EDGE_CURVE ( 'NONE', #9726, #8808, #7578, .T. ) ;
#6615 = FACE_OUTER_BOUND ( 'NONE', #8714, .T. ) ;
#6616 = ADVANCED_BREP_SHAPE_REPRESENTATION ( '', ( #563, #12337 ), #9054 ) ;
#6617 = DIRECTION ( 'NONE',  ( 0.000000000000000000, 0.000000000000000000, -1.000000000000000000 ) ) ;
#6618 = VERTEX_POINT ( 'NONE', #8386 ) ;
#6619 = CIRCLE ( 'NONE', #2054, 3.499999999999999556 ) ;
#6620 = DIRECTION ( 'NONE',  ( 1.000000000000000000, 0.000000000000000000, 0.000000000000000000 ) ) ;
#6621 = CARTESIAN_POINT ( 'NONE',  ( -188.3680287392151627, 131.4989828868489781, 10.16010209732750269 ) ) ;
#6622 = FACE_OUTER_BOUND ( 'NONE', #4735, .T. ) ;
#6623 = AXIS2_PLACEMENT_3D ( 'NONE', #4013, #8847, #10984 ) ;
#6624 = CARTESIAN_POINT ( 'NONE',  ( -156.4041773974485920, 111.1759743691806648, -4.957866620889592291 ) ) ;
#6625 = ORIENTED_EDGE ( 'NONE', *, *, #9348, .F. ) ;
#6626 = ADVANCED_FACE ( 'NONE', ( #4726 ), #4194, .F. ) ;
#6627 = CARTESIAN_POINT ( 'NONE',  ( 190.0000000000000568, -179.8058001507315566, -17.50000000000002487 ) ) ;
#6628 = ORIENTED_EDGE ( 'NONE', *, *, #8851, .F. ) ;
#6629 = ORIENTED_EDGE ( 'NONE', *, *, #5726, .T. ) ;
#6630 = DIRECTION ( 'NONE',  ( -1.000000000000000000, 0.000000000000000000, 0.000000000000000000 ) ) ;
#6631 = CARTESIAN_POINT ( 'NONE',  ( -10.39230484541326582, 4.570335331080236228E-16, 0.000000000000000000 ) ) ;
#6632 = ADVANCED_FACE ( 'NONE', ( #8011 ), #5555, .F. ) ;
#6633 = FILL_AREA_STYLE_COLOUR ( '', #6666 ) ;
#6634 = DIRECTION ( 'NONE',  ( 0.000000000000000000, 0.000000000000000000, 1.000000000000000000 ) ) ;
#6635 = PRODUCT_DEFINITION ( 'UNKNOWN', '', #1721, #6785 ) ;
#6636 = CIRCLE ( 'NONE', #3340, 0.4999999999999996114 ) ;
#6637 = CARTESIAN_POINT ( 'NONE',  ( -216.9798112490933306, 154.4040521289827836, -0.4892415239726802256 ) ) ;
#6638 = EDGE_CURVE ( 'NONE', #2150, #12939, #2519, .T. ) ;
#6639 = DIRECTION ( 'NONE',  ( -1.000000000000000000, -0.000000000000000000, -0.000000000000000000 ) ) ;
#6640 = VECTOR ( 'NONE', #15603, 1000.000000000000000 ) ;
#6641 = DIRECTION ( 'NONE',  ( 0.000000000000000000, 0.1391731009600660485, -0.9902680687415702510 ) ) ;
#6642 = FACE_OUTER_BOUND ( 'NONE', #1930, .T. ) ;
#6643 = CARTESIAN_POINT ( 'NONE',  ( 198.8634854004546071, 49.55149448133588663, -6.680369717582868461 ) ) ;
#6644 = CARTESIAN_POINT ( 'NONE',  ( -169.8702492482470632, 111.5724338074144413, 2.431557144026070372 ) ) ;
#6645 = ORIENTED_EDGE ( 'NONE', *, *, #12136, .T. ) ;
#6646 = CARTESIAN_POINT ( 'NONE',  ( -218.7420931059136251, 151.3070553729347978, 9.190923517782497498 ) ) ;
#6647 = ORIENTED_EDGE ( 'NONE', *, *, #3952, .T. ) ;
#6648 = DIRECTION ( 'NONE',  ( -0.000000000000000000, -0.000000000000000000, 1.000000000000000000 ) ) ;
#6649 = DIRECTION ( 'NONE',  ( 0.000000000000000000, 0.000000000000000000, -1.000000000000000000 ) ) ;
#6650 = EDGE_CURVE ( 'NONE', #11835, #15158, #3779, .T. ) ;
#6651 = ADVANCED_FACE ( 'NONE', ( #6902 ), #5630, .T. ) ;
#6652 = ORIENTED_EDGE ( 'NONE', *, *, #10394, .F. ) ;
#6653 = EDGE_CURVE ( 'NONE', #9261, #3488, #5557, .T. ) ;
#6654 = LINE ( 'NONE', #13730, #12206 ) ;
#6655 = CARTESIAN_POINT ( 'NONE',  ( 122.5806775638430253, 45.00321902537314145, 7.600000000000002309 ) ) ;
#6656 = AXIS2_PLACEMENT_3D ( 'NONE', #13318, #9712, #14426 ) ;
#6657 = DIRECTION ( 'NONE',  ( 1.000000000000000000, 0.000000000000000000, 0.000000000000000000 ) ) ;
#6658 = ORIENTED_EDGE ( 'NONE', *, *, #3215, .T. ) ;
#6659 = ITEM_DEFINED_TRANSFORMATION ( 'NONE', 'NONE', #12315,  #12337 ) ;
#6660 = VERTEX_POINT ( 'NONE', #11635 ) ;
#6661 = AXIS2_PLACEMENT_3D ( 'NONE', #13881, #674, #6784 ) ;
#6662 = DIRECTION ( 'NONE',  ( 1.000000000000000000, 0.000000000000000000, 0.000000000000000000 ) ) ;
#6663 = ORIENTED_EDGE ( 'NONE', *, *, #5376, .F. ) ;
#6664 = LINE ( 'NONE', #13817, #629 ) ;
#6665 = ADVANCED_FACE ( 'NONE', ( #13166 ), #10448, .F. ) ;
#6666 = COLOUR_RGB ( '', 0.09019608, 0.27058824, 0.51372549) ;
#6667 = FACE_OUTER_BOUND ( 'NONE', #6258, .T. ) ;
#6668 = ORIENTED_EDGE ( 'NONE', *, *, #14429, .F. ) ;
#6669 = ORIENTED_EDGE ( 'NONE', *, *, #10791, .T. ) ;
#6670 = CYLINDRICAL_SURFACE ( 'NONE', #9553, 10.97218105532926558 ) ;
#6671 = ORIENTED_EDGE ( 'NONE', *, *, #11293, .F. ) ;
#6672 = CARTESIAN_POINT ( 'NONE',  ( 193.1007612367029367, 46.15997280778478995, -6.307360761128419036 ) ) ;
#6673 = CARTESIAN_POINT ( 'NONE',  ( 15.70000000000004015, 62.13993994372673768, 15.00000000000104983 ) ) ;
#6674 = AXIS2_PLACEMENT_3D ( 'NONE', #7020, #11828, #11905 ) ;
#6675 = CARTESIAN_POINT ( 'NONE',  ( -33.09899788034579871, 48.72489408690345414, 5.000000000000000000 ) ) ;
#6676 = CARTESIAN_POINT ( 'NONE',  ( 50.57199999999998852, 0.000000000000000000, 5.000000000000017764 ) ) ;
#6677 = DIRECTION ( 'NONE',  ( 1.000000000000000000, 0.000000000000000000, 0.000000000000000000 ) ) ;
#6678 = VECTOR ( 'NONE', #8900, 1000.000000000000000 ) ;
#6679 = CARTESIAN_POINT ( 'NONE',  ( 190.0000000000000853, -179.8058001507315566, 65.31842631998698323 ) ) ;
#6680 = ADVANCED_FACE ( 'NONE', ( #8095 ), #12880, .T. ) ;
#6681 = ORIENTED_EDGE ( 'NONE', *, *, #14529, .T. ) ;
#6682 = CARTESIAN_POINT ( 'NONE',  ( 177.5000000000000853, -178.8058001507315566, -18.19066787724516843 ) ) ;
#6683 = TOROIDAL_SURFACE ( 'NONE', #5407, 6.999999999999991118, 2.000000000000000000 ) ;
#6684 = CARTESIAN_POINT ( 'NONE',  ( -219.4290858278833980, 154.0975609761335932, -2.973479603620232226 ) ) ;
#6685 = DIRECTION ( 'NONE',  ( -1.000000000000000000, -2.751328491981765035E-32, 3.965082230804130220E-16 ) ) ;
#6686 = ORIENTED_EDGE ( 'NONE', *, *, #14018, .T. ) ;
#6687 = CARTESIAN_POINT ( 'NONE',  ( -214.6152097961127367, 135.6358893629490581, -0.4555467707853336767 ) ) ;
#6688 = CARTESIAN_POINT ( 'NONE',  ( 211.9100270530500154, 42.38063601863193242, 0.1257832527464326222 ) ) ;
#6689 = ORIENTED_EDGE ( 'NONE', *, *, #8483, .F. ) ;
#6690 = CARTESIAN_POINT ( 'NONE',  ( -64.00000000000002842, 15.53993994372673981, 10.05257423913146475 ) ) ;
#6691 = FACE_OUTER_BOUND ( 'NONE', #2038, .T. ) ;
#6692 = CYLINDRICAL_SURFACE ( 'NONE', #12862, 1.699999999999993072 ) ;
#6693 = CIRCLE ( 'NONE', #3147, 1.499999999999994449 ) ;
#6694 = ADVANCED_FACE ( 'NONE', ( #11713 ), #12646, .T. ) ;
#6695 = DIRECTION ( 'NONE',  ( 0.000000000000000000, 0.000000000000000000, -1.000000000000000000 ) ) ;
#6696 = EDGE_CURVE ( 'NONE', #10652, #12061, #9588, .T. ) ;
#6697 = ORIENTED_EDGE ( 'NONE', *, *, #3533, .T. ) ;
#6698 = DIRECTION ( 'NONE',  ( 0.8950274278067241740, -0.4460111024107797362, 0.000000000000000000 ) ) ;
#6699 = CARTESIAN_POINT ( 'NONE',  ( -207.1471226269450767, 137.0919095985319132, 9.577123744044238052 ) ) ;
#6700 = DIRECTION ( 'NONE',  ( -1.000000000000000000, 0.000000000000000000, 0.000000000000000000 ) ) ;
#6701 = DIRECTION ( 'NONE',  ( 0.000000000000000000, -0.8660254037844380415, 0.5000000000000012212 ) ) ;
#6702 = ORIENTED_EDGE ( 'NONE', *, *, #4517, .T. ) ;
#6703 = CARTESIAN_POINT ( 'NONE',  ( -172.2688154150754940, 113.4305367422061579, 5.000000000000000000 ) ) ;
#6704 = VECTOR ( 'NONE', #2960, 1000.000000000000000 ) ;
#6705 = ORIENTED_EDGE ( 'NONE', *, *, #4008, .T. ) ;
#6706 = VERTEX_POINT ( 'NONE', #6675 ) ;
#6707 = CARTESIAN_POINT ( 'NONE',  ( -144.0627431139473345, 95.36268816863731956, 0.000000000000000000 ) ) ;
#6708 = CARTESIAN_POINT ( 'NONE',  ( 14.00000000000004086, 64.53993994372673626, 11.47500000000104947 ) ) ;
#6709 = ADVANCED_FACE ( 'NONE', ( #11479 ), #2782, .F. ) ;
#6710 = CARTESIAN_POINT ( 'NONE',  ( -174.2842449426172209, 115.9750891085876390, 2.645078463637116073 ) ) ;
#6711 = CARTESIAN_POINT ( 'NONE',  ( -219.8521491127885383, 153.3395766914946421, -3.516840477861103320 ) ) ;
#6712 = LINE ( 'NONE', #10178, #2159 ) ;
#6713 = VECTOR ( 'NONE', #9899, 1000.000000000000000 ) ;
#6714 = LINE ( 'NONE', #5441, #2097 ) ;
#6715 = PLANE ( 'NONE',  #5397 ) ;
#6716 = VECTOR ( 'NONE', #2325, 1000.000000000000000 ) ;
#6717 = EDGE_CURVE ( 'NONE', #15368, #12236, #14563, .T. ) ;
#6718 = DIRECTION ( 'NONE',  ( -1.000000000000000000, 0.000000000000000000, 0.000000000000000000 ) ) ;
#6719 = CARTESIAN_POINT ( 'NONE',  ( -220.2506544535641524, 152.6255918187081875, -1.607790317205930686 ) ) ;
#6720 = EDGE_LOOP ( 'NONE', ( #12103, #7767, #7382, #1222 ) ) ;
#6721 = ORIENTED_EDGE ( 'NONE', *, *, #3750, .T. ) ;
#6722 = LINE ( 'NONE', #13802, #11076 ) ;
#6723 = DIRECTION ( 'NONE',  ( -0.000000000000000000, -0.000000000000000000, 1.000000000000000000 ) ) ;
#6724 = LINE ( 'NONE', #11527, #297 ) ;
#6725 = DIRECTION ( 'NONE',  ( 1.000000000000000000, -0.000000000000000000, -0.000000000000000000 ) ) ;
#6726 = LINE ( 'NONE', #11690, #15374 ) ;
#6727 = CIRCLE ( 'NONE', #5204, 3.500000000000004885 ) ;
#6728 = FACE_OUTER_BOUND ( 'NONE', #568, .T. ) ;
#6729 = ORIENTED_EDGE ( 'NONE', *, *, #3664, .F. ) ;
#6730 = ORIENTED_EDGE ( 'NONE', *, *, #338, .F. ) ;
#6731 = EDGE_CURVE ( 'NONE', #2171, #868, #5043, .T. ) ;
#6732 = CARTESIAN_POINT ( 'NONE',  ( 209.5364819485449175, 48.08777744531177945, -8.760749929847346351 ) ) ;
#6734 = EDGE_CURVE ( 'NONE', #14322, #7924, #9948, .T. ) ;
#6733 = ADVANCED_FACE ( 'NONE', ( #10902 ), #9714, .T. ) ;
#6735 = EDGE_LOOP ( 'NONE', ( #11120, #3646, #13717, #12166, #3560 ) ) ;
#6736 = AXIS2_PLACEMENT_3D ( 'NONE', #8685, #10024, #2917 ) ;
#6737 = FACE_OUTER_BOUND ( 'NONE', #10518, .T. ) ;
#6738 = CARTESIAN_POINT ( 'NONE',  ( -223.6165645121877503, 142.0072334165735981, 2.089048013359927847 ) ) ;
#6739 = VERTEX_POINT ( 'NONE', #2679 ) ;
#6740 = EDGE_LOOP ( 'NONE', ( #11161, #2368, #6319, #3311, #8429, #5755 ) ) ;
#6741 = CARTESIAN_POINT ( 'NONE',  ( 71.96535645333923981, 38.79159067395544014, 5.000000000000000000 ) ) ;
#6742 = CARTESIAN_POINT ( 'NONE',  ( -63.50000000000002842, 19.53993994372674692, -17.50000000000002487 ) ) ;
#6743 = ORIENTED_EDGE ( 'NONE', *, *, #44, .T. ) ;
#6744 = CARTESIAN_POINT ( 'NONE',  ( 194.7691866843436799, 33.87697957786221536, -2.559886773443665220 ) ) ;
#6745 = CARTESIAN_POINT ( 'NONE',  ( -76.00000000000001421, 15.03993994372673804, 24.94742576086838781 ) ) ;
#6746 = CARTESIAN_POINT ( 'NONE',  ( 207.1062858801516597, 40.86394065090267702, 16.00000000000001421 ) ) ;
#6747 = CARTESIAN_POINT ( 'NONE',  ( -35.99999999999995026, 64.53993994372673626, 15.00000000000139977 ) ) ;
#6748 = CARTESIAN_POINT ( 'NONE',  ( 64.00000000000005684, 64.53993994372673626, 15.00000000000070166 ) ) ;
#6749 = DIRECTION ( 'NONE',  ( 1.000000000000000000, -0.000000000000000000, -0.000000000000000000 ) ) ;
#6750 = EDGE_LOOP ( 'NONE', ( #8470, #13640, #14801, #4601 ) ) ;
#6751 = FACE_OUTER_BOUND ( 'NONE', #15117, .T. ) ;
#6752 = CARTESIAN_POINT ( 'NONE',  ( -172.3538414453648500, 130.1468270526879110, 1.515441478062062641 ) ) ;
#6753 = PLANE ( 'NONE',  #1745 ) ;
#6754 = ORIENTED_EDGE ( 'NONE', *, *, #14372, .T. ) ;
#6755 = CARTESIAN_POINT ( 'NONE',  ( -171.9831566630682858, 119.3897064310878875, -4.822481523602708542 ) ) ;
#6756 = UNCERTAINTY_MEASURE_WITH_UNIT (LENGTH_MEASURE( 1.000000000000000082E-05 ), #5353, 'distance_accuracy_value', 'NONE');
#6757 = CARTESIAN_POINT ( 'NONE',  ( 188.3378656401271201, 39.26133998289535043, -1.370343197488200548 ) ) ;
#6758 = ORIENTED_EDGE ( 'NONE', *, *, #3337, .F. ) ;
#6759 = FACE_OUTER_BOUND ( 'NONE', #3736, .T. ) ;
#6760 = CARTESIAN_POINT ( 'NONE',  ( 17.41029453487719181, 40.04259805664093363, 10.00000000000000178 ) ) ;
#6761 = CARTESIAN_POINT ( 'NONE',  ( -151.1262866895993966, 106.2783261085441495, -4.449251264896262548 ) ) ;
#6762 = EDGE_CURVE ( 'NONE', #1955, #2689, #13551, .T. ) ;
#6763 = VECTOR ( 'NONE', #6861, 1000.000000000000114 ) ;
#6764 = AXIS2_PLACEMENT_3D ( 'NONE', #8219, #6869, #10722 ) ;
#6765 = DIRECTION ( 'NONE',  ( -0.000000000000000000, 0.000000000000000000, 1.000000000000000000 ) ) ;
#6766 = ORIENTED_EDGE ( 'NONE', *, *, #9676, .T. ) ;
#6767 = FACE_OUTER_BOUND ( 'NONE', #6108, .T. ) ;
#6768 = CARTESIAN_POINT ( 'NONE',  ( -208.4006302466032992, 134.8330880460140122, 7.918248976830637886 ) ) ;
#6769 = DIRECTION ( 'NONE',  ( 0.000000000000000000, 0.000000000000000000, 1.000000000000000000 ) ) ;
#6770 = DIRECTION ( 'NONE',  ( -0.7900120431063429871, 0.6130913241491365850, 0.000000000000000000 ) ) ;
#6771 = PRODUCT_DEFINITION_SHAPE ( 'NONE', 'NONE',  #15623 ) ;
#6772 = ORIENTED_EDGE ( 'NONE', *, *, #13850, .F. ) ;
#6773 = DIRECTION ( 'NONE',  ( -1.000000000000000000, 0.000000000000000000, -0.000000000000000000 ) ) ;
#6774 = CIRCLE ( 'NONE', #1203, 0.5000000000000004441 ) ;
#6775 = EDGE_LOOP ( 'NONE', ( #3171, #3472 ) ) ;
#6776 = ORIENTED_EDGE ( 'NONE', *, *, #14718, .F. ) ;
#6777 = DIRECTION ( 'NONE',  ( 0.000000000000000000, -1.000000000000000000, -1.156482317317871478E-16 ) ) ;
#6778 = CARTESIAN_POINT ( 'NONE',  ( 190.0000000000000568, -178.8058001507315566, 53.19066787724494816 ) ) ;
#6779 = CARTESIAN_POINT ( 'NONE',  ( 2.000000000000000000, 3.175426480542944407, 0.000000000000000000 ) ) ;
#6780 = CARTESIAN_POINT ( 'NONE',  ( -173.3690302610533251, 117.6148398750801789, 7.519404742434161903 ) ) ;
#6781 = EDGE_CURVE ( 'NONE', #61, #12693, #11047, .T. ) ;
#6782 = CARTESIAN_POINT ( 'NONE',  ( -221.5356353662852200, 150.3233468055901767, -2.966311635581158956 ) ) ;
#6783 = FACE_OUTER_BOUND ( 'NONE', #9493, .T. ) ;
#6784 = DIRECTION ( 'NONE',  ( 1.000000000000000000, 0.000000000000000000, 0.000000000000000000 ) ) ;
#6785 = PRODUCT_DEFINITION_CONTEXT ( 'detailed design', #713, 'design' ) ;
#6786 = ORIENTED_EDGE ( 'NONE', *, *, #5460, .F. ) ;
#6787 = DIRECTION ( 'NONE',  ( 0.000000000000000000, 0.000000000000000000, 1.000000000000000000 ) ) ;
#6788 = LINE ( 'NONE', #6947, #12203 ) ;
#6789 = CARTESIAN_POINT ( 'NONE',  ( -64.00000000000002842, 15.03993994372673804, 24.94742576086838781 ) ) ;
#6790 = CARTESIAN_POINT ( 'NONE',  ( -85.27455057502459113, 65.19100426474074084, 0.000000000000000000 ) ) ;
#6791 = ORIENTED_EDGE ( 'NONE', *, *, #14042, .T. ) ;
#6792 = CARTESIAN_POINT ( 'NONE',  ( -218.4677351830674183, 155.8199715629180275, 3.280001329119076825 ) ) ;
#6793 = ORIENTED_EDGE ( 'NONE', *, *, #15180, .F. ) ;
#6794 = DIRECTION ( 'NONE',  ( 1.000000000000000000, 0.000000000000000000, 0.000000000000000000 ) ) ;
#6795 = CYLINDRICAL_SURFACE ( 'NONE', #14895, 3.500000000000003109 ) ;
#6796 = EDGE_LOOP ( 'NONE', ( #9087, #8271, #8718, #11957 ) ) ;
#6797 = CARTESIAN_POINT ( 'NONE',  ( -213.7073284247934453, 153.2176779349464368, 2.500000000000000000 ) ) ;
#6798 = CARTESIAN_POINT ( 'NONE',  ( 166.7445055987502656, 66.43865443379108626, -0.9107274384406879308 ) ) ;
#6799 = VECTOR ( 'NONE', #15537, 1000.000000000000000 ) ;
#6800 = AXIS2_PLACEMENT_3D ( 'NONE', #12807, #1996, #5788 ) ;
#6801 = ADVANCED_FACE ( 'NONE', ( #14740 ), #7501, .F. ) ;
#6802 = DIRECTION ( 'NONE',  ( 1.000000000000000000, 0.000000000000000000, 0.000000000000000000 ) ) ;
#6803 = ORIENTED_EDGE ( 'NONE', *, *, #6164, .T. ) ;
#6804 = AXIS2_PLACEMENT_3D ( 'NONE', #566, #12723, #7865 ) ;
#6805 = VERTEX_POINT ( 'NONE', #3626 ) ;
#6806 = AXIS2_PLACEMENT_3D ( 'NONE', #4292, #10384, #10309 ) ;
#6807 = CARTESIAN_POINT ( 'NONE',  ( 198.5455061167297117, 29.08454594588317477, -3.885748181069116569 ) ) ;
#6808 = DIRECTION ( 'NONE',  ( 0.000000000000000000, 1.000000000000000000, 0.000000000000000000 ) ) ;
#6809 = ORIENTED_EDGE ( 'NONE', *, *, #11499, .F. ) ;
#6810 = DIRECTION ( 'NONE',  ( 5.518327896226373307E-17, 0.9902680687415712502, 0.1391731009600586100 ) ) ;
#6811 = CARTESIAN_POINT ( 'NONE',  ( -85.27455057502459113, 65.19100426474074084, 10.00000000000000178 ) ) ;
#6812 = EDGE_LOOP ( 'NONE', ( #10342, #5215, #10858, #11371 ) ) ;
#6813 = EDGE_LOOP ( 'NONE', ( #15300, #13743, #7356, #4586 ) ) ;
#6814 = LINE ( 'NONE', #15157, #7794 ) ;
#6815 = EDGE_CURVE ( 'NONE', #3946, #649, #11337, .T. ) ;
#6816 = DIRECTION ( 'NONE',  ( -0.05388311488299379198, -0.09654005853512973023, 0.9938695221348423647 ) ) ;
#6817 = ORIENTED_EDGE ( 'NONE', *, *, #13914, .F. ) ;
#6818 = CARTESIAN_POINT ( 'NONE',  ( 207.1288103955774318, 46.12660085639766550, -4.186765234109192768 ) ) ;
#6819 = CARTESIAN_POINT ( 'NONE',  ( -5.196152422706636465, 9.000000000000001776, 5.000000000000000000 ) ) ;
#6820 = AXIS2_PLACEMENT_3D ( 'NONE', #3373, #8441, #4628 ) ;
#6821 = AXIS2_PLACEMENT_3D ( 'NONE', #14493, #5907, #7261 ) ;
#6822 = DIRECTION ( 'NONE',  ( -1.224646799147353207E-16, 1.000000000000000000, 0.000000000000000000 ) ) ;
#6823 = DIRECTION ( 'NONE',  ( 0.000000000000000000, 1.000000000000000000, 6.938893903907227145E-17 ) ) ;
#6824 = EDGE_CURVE ( 'NONE', #12658, #12750, #11604, .T. ) ;
#6825 = CARTESIAN_POINT ( 'NONE',  ( 21.99999999999999289, 0.000000000000000000, 1.219500000000000028 ) ) ;
#6826 = ADVANCED_FACE ( 'NONE', ( #287 ), #4793, .F. ) ;
#6827 = FACE_OUTER_BOUND ( 'NONE', #6813, .T. ) ;
#6828 = AXIS2_PLACEMENT_3D ( 'NONE', #1342, #8546, #13258 ) ;
#6829 = ORIENTED_EDGE ( 'NONE', *, *, #6359, .T. ) ;
#6830 = DIRECTION ( 'NONE',  ( -0.000000000000000000, 1.000000000000000000, -0.000000000000000000 ) ) ;
#6831 = CIRCLE ( 'NONE', #7600, 1.499999999999997780 ) ;
#6832 = CARTESIAN_POINT ( 'NONE',  ( -177.3513212993587729, 132.9361332244957055, 1.515441477536284109 ) ) ;
#6833 = AXIS2_PLACEMENT_3D ( 'NONE', #181, #4953, #7335 ) ;
#6834 = FACE_OUTER_BOUND ( 'NONE', #11618, .T. ) ;
#6835 = ORIENTED_EDGE ( 'NONE', *, *, #895, .T. ) ;
#6836 = CARTESIAN_POINT ( 'NONE',  ( -170.7063108826370694, 121.6823135672476752, -5.361935827173478941 ) ) ;
#6837 = CARTESIAN_POINT ( 'NONE',  ( 201.6895650671498288, 29.08490409614774208, -0.6212496039192949571 ) ) ;
#6838 = ORIENTED_EDGE ( 'NONE', *, *, #2084, .F. ) ;
#6839 = EDGE_CURVE ( 'NONE', #12197, #158, #8757, .T. ) ;
#6840 = DIRECTION ( 'NONE',  ( 0.000000000000000000, 0.000000000000000000, -1.000000000000000000 ) ) ;
#6841 = CARTESIAN_POINT ( 'NONE',  ( -85.99999999999994316, 64.51493994372674479, 15.00000000000174794 ) ) ;
#6842 = EDGE_CURVE ( 'NONE', #13988, #7301, #15609, .T. ) ;
#6843 = CIRCLE ( 'NONE', #4550, 1.000000000000000000 ) ;
#6844 = CARTESIAN_POINT ( 'NONE',  ( -152.3062201278460748, 106.7562614988853369, -4.377525546821595448 ) ) ;
#6845 = VECTOR ( 'NONE', #2101, 1000.000000000000000 ) ;
#6846 = EDGE_LOOP ( 'NONE', ( #13141, #10480, #3449, #4506, #1769, #6350 ) ) ;
#6847 = CARTESIAN_POINT ( 'NONE',  ( 0.000000000000000000, 0.000000000000000000, 0.000000000000000000 ) ) ;
#6848 = FACE_OUTER_BOUND ( 'NONE', #13888, .T. ) ;
#6849 = ORIENTED_EDGE ( 'NONE', *, *, #14018, .F. ) ;
#6850 = CARTESIAN_POINT ( 'NONE',  ( -63.50000000000002842, 19.53993994372673626, 52.49999999999997868 ) ) ;
#6851 = CARTESIAN_POINT ( 'NONE',  ( -222.1166800156826184, 149.2823141075699880, 10.12588066961105504 ) ) ;
#6852 = CARTESIAN_POINT ( 'NONE',  ( 190.0000000000000568, 14.97035339324670922, -2.580050169239785696 ) ) ;
#6853 = CARTESIAN_POINT ( 'NONE',  ( 0.1306530452038093260, 7.903938623646864059, 2.309976723937613663 ) ) ;
#6854 = EDGE_LOOP ( 'NONE', ( #1504, #11384, #10934, #13290 ) ) ;
#6855 = CIRCLE ( 'NONE', #9131, 1.699999999999993072 ) ;
#6856 = EDGE_CURVE ( 'NONE', #1071, #4418, #12347, .T. ) ;
#6857 = EDGE_LOOP ( 'NONE', ( #11428, #9594, #13314 ) ) ;
#6858 = ORIENTED_EDGE ( 'NONE', *, *, #10829, .T. ) ;
#6859 = VECTOR ( 'NONE', #6281, 1000.000000000000000 ) ;
#6860 = LINE ( 'NONE', #11671, #12359 ) ;
#6861 = DIRECTION ( 'NONE',  ( 0.5000000000000001110, -0.8660254037844385966, 0.000000000000000000 ) ) ;
#6862 = CYLINDRICAL_SURFACE ( 'NONE', #6905, 3.500000000000004885 ) ;
#6863 = CARTESIAN_POINT ( 'NONE',  ( -174.1472389072507383, 116.2205569272661734, 4.466624464644515236 ) ) ;
#6864 = CARTESIAN_POINT ( 'NONE',  ( -224.4909276189729894, 145.0284768322981108, -3.162994880121249963 ) ) ;
#6865 = CARTESIAN_POINT ( 'NONE',  ( 203.4093511297053851, 50.30250970312692971, -0.9107274384406970347 ) ) ;
#6866 = VECTOR ( 'NONE', #7197, 1000.000000000000114 ) ;
#6867 = DIRECTION ( 'NONE',  ( 0.000000000000000000, -1.000000000000000000, -1.156482317317871478E-16 ) ) ;
#6868 = CIRCLE ( 'NONE', #2582, 1.000000000000000888 ) ;
#6869 = DIRECTION ( 'NONE',  ( 0.000000000000000000, 0.000000000000000000, -1.000000000000000000 ) ) ;
#6870 = CARTESIAN_POINT ( 'NONE',  ( -63.50000000000002842, -178.8058001507315566, -18.19066787724516843 ) ) ;
#6871 = CARTESIAN_POINT ( 'NONE',  ( -76.50000000000001421, 19.53993994372674692, -17.50000000000002487 ) ) ;
#6872 = ADVANCED_FACE ( 'NONE', ( #13404 ), #14431, .F. ) ;
#6873 = CARTESIAN_POINT ( 'NONE',  ( -64.00000000000002842, 15.03993994372673981, -3.075184203610571654 ) ) ;
#6874 = ORIENTED_EDGE ( 'NONE', *, *, #13202, .F. ) ;
#6875 = EDGE_LOOP ( 'NONE', ( #8779, #5348, #7994, #8868, #8910, #1593, #2367, #2377, #15320, #13256, #12084, #5427, #7001, #5795 ) ) ;
#6876 = PLANE ( 'NONE',  #11039 ) ;
#6877 = CARTESIAN_POINT ( 'NONE',  ( -216.6980668629938123, 154.8869363267023687, 2.500000000158653091 ) ) ;
#6878 = CIRCLE ( 'NONE', #9894, 0.9999999999999991118 ) ;
#6879 = ORIENTED_EDGE ( 'NONE', *, *, #3740, .F. ) ;
#6880 = CARTESIAN_POINT ( 'NONE',  ( -201.8658614229783268, 146.6084512934502584, 2.500000000000000000 ) ) ;
#6881 = CARTESIAN_POINT ( 'NONE',  ( -64.00000000000002842, -179.8058001507315566, -51.45141194869119516 ) ) ;
#6882 = CLOSED_SHELL ( 'NONE', ( #15576, #15604, #3782, #717, #4981, #8903, #6933, #1962, #7840 ) ) ;
#6883 = DIRECTION ( 'NONE',  ( 0.000000000000000000, 0.000000000000000000, -1.000000000000000000 ) ) ;
#6884 = ORIENTED_EDGE ( 'NONE', *, *, #12857, .F. ) ;
#6885 = ADVANCED_FACE ( 'NONE', ( #7428 ), #2441, .T. ) ;
#6886 = ITEM_DEFINED_TRANSFORMATION ( 'NONE', 'NONE', #2228,  #12337 ) ;
#6887 = VERTEX_POINT ( 'NONE', #8686 ) ;
#6888 = CARTESIAN_POINT ( 'NONE',  ( 207.4341467637200651, 31.47497422714618764, -9.505705820141434614 ) ) ;
#6889 = DIRECTION ( 'NONE',  ( -0.000000000000000000, -0.000000000000000000, 1.000000000000000000 ) ) ;
#6890 = ORIENTED_EDGE ( 'NONE', *, *, #2606, .F. ) ;
#6891 = DIRECTION ( 'NONE',  ( 1.000000000000000000, 0.000000000000000000, 0.000000000000000000 ) ) ;
#6892 = CARTESIAN_POINT ( 'NONE',  ( 164.0000000000000568, 64.53993994372673626, 15.00000000000000355 ) ) ;
#6893 = CARTESIAN_POINT ( 'NONE',  ( 178.0000000000000853, -178.6666270497714777, 53.18093594598651919 ) ) ;
#6894 = ORIENTED_EDGE ( 'NONE', *, *, #13184, .F. ) ;
#6895 = ORIENTED_EDGE ( 'NONE', *, *, #1702, .T. ) ;
#6896 = CARTESIAN_POINT ( 'NONE',  ( 178.0000000000000853, -179.3058001507315566, -29.88378295107905913 ) ) ;
#6897 = EDGE_CURVE ( 'NONE', #13949, #11700, #12850, .T. ) ;
#6898 = COLOUR_RGB ( '', 0.72549020, 0.75294118, 0.79215686) ;
#6899 = VERTEX_POINT ( 'NONE', #6161 ) ;
#6900 = LINE ( 'NONE', #4355, #8344 ) ;
#6901 = EDGE_CURVE ( 'NONE', #9730, #163, #13321, .T. ) ;
#6902 = FACE_OUTER_BOUND ( 'NONE', #9369, .T. ) ;
#6903 = CARTESIAN_POINT ( 'NONE',  ( 200.1062858801516597, 40.86394065090267702, -219.0000000000000853 ) ) ;
#6904 = AXIS2_PLACEMENT_3D ( 'NONE', #15208, #2114, #15278 ) ;
#6905 = AXIS2_PLACEMENT_3D ( 'NONE', #12920, #15350, #2107 ) ;
#6906 = ORIENTED_EDGE ( 'NONE', *, *, #8613, .T. ) ;
#6907 = FACE_OUTER_BOUND ( 'NONE', #6963, .T. ) ;
#6908 = EDGE_CURVE ( 'NONE', #14048, #1178, #1244, .T. ) ;
#6909 = CARTESIAN_POINT ( 'NONE',  ( -208.4264987254875052, 144.6230976266233483, -4.640918829492436615 ) ) ;
#6910 = LINE ( 'NONE', #10691, #1233 ) ;
#6911 = ORIENTED_EDGE ( 'NONE', *, *, #3852, .F. ) ;
#6912 = CARTESIAN_POINT ( 'NONE',  ( -204.9433645127610646, 133.1096489332827275, -2.964974570226844186 ) ) ;
#6913 = UNCERTAINTY_MEASURE_WITH_UNIT (LENGTH_MEASURE( 1.000000000000000082E-05 ), #248, 'distance_accuracy_value', 'NONE');
#6914 = CARTESIAN_POINT ( 'NONE',  ( 211.8731694863154758, 39.16394563883312685, -2.997139605818726515 ) ) ;
#6915 = TOROIDAL_SURFACE ( 'NONE', #1347, 1.000000000000000000, 0.5000000000000000000 ) ;
#6916 = ORIENTED_EDGE ( 'NONE', *, *, #14912, .T. ) ;
#6917 = CIRCLE ( 'NONE', #6165, 3.500000000000003109 ) ;
#6918 = PLANE ( 'NONE',  #8325 ) ;
#6919 = CYLINDRICAL_SURFACE ( 'NONE', #5942, 1.700000000000000178 ) ;
#6920 = CARTESIAN_POINT ( 'NONE',  ( 0.000000000000000000, 0.000000000000000000, 5.000000000000000000 ) ) ;
#6921 = AXIS2_PLACEMENT_3D ( 'NONE', #12677, #3372, #8132 ) ;
#6922 = EDGE_LOOP ( 'NONE', ( #12705, #5023, #1877, #2705 ) ) ;
#6923 = VECTOR ( 'NONE', #12926, 1000.000000000000000 ) ;
#6924 =( NAMED_UNIT ( * ) SI_UNIT ( $, .STERADIAN. ) SOLID_ANGLE_UNIT ( ) );
#6925 = CYLINDRICAL_SURFACE ( 'NONE', #8896, 1.699999999999993072 ) ;
#6926 = ORIENTED_EDGE ( 'NONE', *, *, #5362, .T. ) ;
#6927 = DIRECTION ( 'NONE',  ( 1.000000000000000000, 0.000000000000000000, 0.000000000000000000 ) ) ;
#6928 = EDGE_CURVE ( 'NONE', #12140, #11697, #8839, .T. ) ;
#6929 = CIRCLE ( 'NONE', #7409, 0.5000000000000004441 ) ;
#6930 = EDGE_CURVE ( 'NONE', #1328, #11071, #5286, .T. ) ;
#6931 = CARTESIAN_POINT ( 'NONE',  ( -169.4720549176639395, 123.8986143635366943, 9.496311331651778431 ) ) ;
#6933 = ADVANCED_FACE ( 'NONE', ( #8997 ), #5512, .T. ) ;
#6932 = CARTESIAN_POINT ( 'NONE',  ( 0.000000000000000000, 0.000000000000000000, 5.000000000000000000 ) ) ;
#6934 = DIRECTION ( 'NONE',  ( -0.000000000000000000, 1.000000000000000000, -0.000000000000000000 ) ) ;
#6935 = CARTESIAN_POINT ( 'NONE',  ( 164.0000000000000568, 64.53993994372673626, 15.00000000000000355 ) ) ;
#6936 = ORIENTED_EDGE ( 'NONE', *, *, #12619, .F. ) ;
#6937 = ORIENTED_EDGE ( 'NONE', *, *, #14626, .T. ) ;
#6938 = CYLINDRICAL_SURFACE ( 'NONE', #9595, 1.499999999999994449 ) ;
#6939 = DIRECTION ( 'NONE',  ( 0.000000000000000000, 0.000000000000000000, 1.000000000000000000 ) ) ;
#6940 = VECTOR ( 'NONE', #13211, 1000.000000000000000 ) ;
#6941 = DIRECTION ( 'NONE',  ( 0.000000000000000000, 0.000000000000000000, 1.000000000000000000 ) ) ;
#6942 = CARTESIAN_POINT ( 'NONE',  ( -171.8875587097026028, 120.2691287111299374, 9.563504314567204290 ) ) ;
#6943 = CARTESIAN_POINT ( 'NONE',  ( -220.9930168758324669, 147.0937147668695957, -4.878251604516314899 ) ) ;
#6944 = CARTESIAN_POINT ( 'NONE',  ( -223.6175992062213140, 142.0096542461538718, 2.866221285019154852 ) ) ;
#6945 = CARTESIAN_POINT ( 'NONE',  ( -76.00000000000001421, -178.6666270497714777, -18.18093594598673945 ) ) ;
#6946 = DIRECTION ( 'NONE',  ( 1.000000000000000000, 0.000000000000000000, 0.000000000000000000 ) ) ;
#6947 = CARTESIAN_POINT ( 'NONE',  ( 177.5000000000000853, -179.3058001507315566, 84.88378295107887084 ) ) ;
#6948 = VECTOR ( 'NONE', #15549, 1000.000000000000000 ) ;
#6949 = CARTESIAN_POINT ( 'NONE',  ( 190.5000000000000568, -179.3058001507315566, -30.31842631998718574 ) ) ;
#6950 = DIRECTION ( 'NONE',  ( 0.000000000000000000, -1.000000000000000000, -4.956352788505162775E-17 ) ) ;
#6951 = FACE_OUTER_BOUND ( 'NONE', #12778, .T. ) ;
#6952 = ORIENTED_EDGE ( 'NONE', *, *, #915, .F. ) ;
#6953 = VERTEX_POINT ( 'NONE', #12276 ) ;
#6954 = DIRECTION ( 'NONE',  ( 0.000000000000000000, -0.1391731009600582492, -0.9902680687415713612 ) ) ;
#6955 = CARTESIAN_POINT ( 'NONE',  ( -76.00000000000004263, -179.3058001507315566, 65.31842631998698323 ) ) ;
#6956 = ORIENTED_EDGE ( 'NONE', *, *, #11449, .F. ) ;
#6957 = CARTESIAN_POINT ( 'NONE',  ( 177.5000000000000853, 19.53993994372673626, 52.49999999999997868 ) ) ;
#6958 = CARTESIAN_POINT ( 'NONE',  ( 190.0000000000000568, 15.03993994372673981, 10.05257423913146475 ) ) ;
#6959 = CIRCLE ( 'NONE', #115, 0.5000000000000004441 ) ;
#6960 = ADVANCED_FACE ( 'NONE', ( #14721 ), #8593, .T. ) ;
#6961 = EDGE_LOOP ( 'NONE', ( #15371, #8235, #4871, #7713 ) ) ;
#6962 = EDGE_CURVE ( 'NONE', #2861, #5048, #9770, .T. ) ;
#6963 = EDGE_LOOP ( 'NONE', ( #4186, #13539, #8005, #15456 ) ) ;
#6964 = CARTESIAN_POINT ( 'NONE',  ( 207.3850704934720284, 31.45434786795649984, -6.508326106789642296 ) ) ;
#6965 = DIRECTION ( 'NONE',  ( 1.000000000000000000, 2.751328491981765035E-32, -3.965082230804130220E-16 ) ) ;
#6966 = ORIENTED_EDGE ( 'NONE', *, *, #4197, .F. ) ;
#6967 = DIRECTION ( 'NONE',  ( -0.000000000000000000, 1.000000000000000000, -0.000000000000000000 ) ) ;
#6968 = VECTOR ( 'NONE', #15204, 1000.000000000000000 ) ;
#6969 = CARTESIAN_POINT ( 'NONE',  ( 120.8806775638430224, 45.00321902537314145, 10.00000000000000178 ) ) ;
#6970 = DIRECTION ( 'NONE',  ( 0.9296197478520976665, 0.3660421972118349521, -0.04266420354037676888 ) ) ;
#6971 = VERTEX_POINT ( 'NONE', #10961 ) ;
#6972 = ORIENTED_EDGE ( 'NONE', *, *, #7180, .T. ) ;
#6973 = DIRECTION ( 'NONE',  ( -0.000000000000000000, -0.000000000000000000, 1.000000000000000000 ) ) ;
#6974 = AXIS2_PLACEMENT_3D ( 'NONE', #2400, #4854, #2475 ) ;
#6975 = DIRECTION ( 'NONE',  ( -0.000000000000000000, -0.000000000000000000, -1.000000000000000000 ) ) ;
#6976 = ORIENTED_EDGE ( 'NONE', *, *, #12580, .T. ) ;
#6977 = CARTESIAN_POINT ( 'NONE',  ( -152.4086188282879561, 107.1438406965016554, 9.367218745794350099 ) ) ;
#6978 = CARTESIAN_POINT ( 'NONE',  ( -85.27455057502459113, 65.19100426474074084, 7.600000000000002309 ) ) ;
#6979 = EDGE_CURVE ( 'NONE', #1838, #12812, #3284, .T. ) ;
#6980 = DIRECTION ( 'NONE',  ( -0.000000000000000000, -0.000000000000000000, 1.000000000000000000 ) ) ;
#6981 = VECTOR ( 'NONE', #2442, 1000.000000000000000 ) ;
#6982 = AXIS2_PLACEMENT_3D ( 'NONE', #11332, #3764, #11029 ) ;
#6983 = ORIENTED_EDGE ( 'NONE', *, *, #11908, .T. ) ;
#6984 = SURFACE_SIDE_STYLE ('',( #8327 ) ) ;
#6985 = ORIENTED_EDGE ( 'NONE', *, *, #13753, .F. ) ;
#6986 = EDGE_CURVE ( 'NONE', #4984, #12099, #15122, .T. ) ;
#6987 = LINE ( 'NONE', #1046, #4670 ) ;
#6988 = CARTESIAN_POINT ( 'NONE',  ( -219.9064123261074428, 153.2423556269449421, 2.431557144026069928 ) ) ;
#6989 = DIRECTION ( 'NONE',  ( 1.000000000000000000, 0.000000000000000000, 0.000000000000000000 ) ) ;
#6990 = VERTEX_POINT ( 'NONE', #13224 ) ;
#6991 = CARTESIAN_POINT ( 'NONE',  ( -175.7369819406991382, 118.3688719364822646, -3.133266157129962259 ) ) ;
#6992 = CARTESIAN_POINT ( 'NONE',  ( 201.3303440367248243, 32.15585396293944598, -6.755036635249508592 ) ) ;
#6993 = VERTEX_POINT ( 'NONE', #9617 ) ;
#6994 = DIRECTION ( 'NONE',  ( 1.000000000000000000, 0.000000000000000000, 0.000000000000000000 ) ) ;
#6995 = CARTESIAN_POINT ( 'NONE',  ( 0.1085346982753684214, -1.064859738956084545, -2.750000000000000444 ) ) ;
#6996 = DIRECTION ( 'NONE',  ( 0.000000000000000000, -1.000000000000000000, 0.000000000000000000 ) ) ;
#6997 = EDGE_CURVE ( 'NONE', #14684, #457, #6068, .T. ) ;
#6998 = VERTEX_POINT ( 'NONE', #8668 ) ;
#6999 = CARTESIAN_POINT ( 'NONE',  ( 193.1265229109121435, 35.50728864820005981, -5.680987958736793075 ) ) ;
#7000 = AXIS2_PLACEMENT_3D ( 'NONE', #4087, #8919, #5354 ) ;
#7001 = ORIENTED_EDGE ( 'NONE', *, *, #895, .F. ) ;
#7002 = DIRECTION ( 'NONE',  ( 1.000000000000000000, 0.000000000000000000, 0.000000000000000000 ) ) ;
#7003 = CARTESIAN_POINT ( 'NONE',  ( -179.3772030532177837, 117.5545944912402661, 1.382365641875445528 ) ) ;
#7004 = LINE ( 'NONE', #9372, #7542 ) ;
#7005 = DIRECTION ( 'NONE',  ( 0.000000000000000000, 0.000000000000000000, 1.000000000000000000 ) ) ;
#7006 = DIRECTION ( 'NONE',  ( -1.000000000000000000, -2.751328491981765035E-32, 3.965082230804130220E-16 ) ) ;
#7007 = ORIENTED_EDGE ( 'NONE', *, *, #5421, .T. ) ;
#7008 = ORIENTED_EDGE ( 'NONE', *, *, #11583, .T. ) ;
#7009 = DIRECTION ( 'NONE',  ( -0.000000000000000000, 1.000000000000000000, 0.000000000000000000 ) ) ;
#7010 = CARTESIAN_POINT ( 'NONE',  ( 5.799999999999999822, 7.999999999999979572, 0.000000000000000000 ) ) ;
#7011 = ADVANCED_FACE ( 'NONE', ( #12202 ), #13460, .F. ) ;
#7012 = LINE ( 'NONE', #6779, #13689 ) ;
#7013 = CARTESIAN_POINT ( 'NONE',  ( 21.99999999999999289, 0.000000000000000000, 0.000000000000000000 ) ) ;
#7014 = CARTESIAN_POINT ( 'NONE',  ( -223.9433292823694046, 146.0095852107350254, -1.211090774047295371 ) ) ;
#7015 = CIRCLE ( 'NONE', #8777, 0.5000000000000000000 ) ;
#7017 = EDGE_CURVE ( 'NONE', #1592, #3135, #14413, .T. ) ;
#7016 = PRODUCT_RELATED_PRODUCT_CATEGORY ( 'part', '', ( #827 ) ) ;
#7018 = EDGE_CURVE ( 'NONE', #13295, #1610, #3609, .T. ) ;
#7019 = CARTESIAN_POINT ( 'NONE',  ( -63.50000000000002842, 17.53993994372674692, -17.50000000000002487 ) ) ;
#7020 = CARTESIAN_POINT ( 'NONE',  ( 178.0000000000000853, -178.8058001507315566, 52.19066787724494816 ) ) ;
#7021 = EDGE_CURVE ( 'NONE', #1333, #11585, #15589, .T. ) ;
#7022 = DIRECTION ( 'NONE',  ( 0.000000000000000000, 0.000000000000000000, -1.000000000000000000 ) ) ;
#7023 = DIRECTION ( 'NONE',  ( -1.000000000000000000, 0.000000000000000000, 0.000000000000000000 ) ) ;
#7024 = VECTOR ( 'NONE', #13629, 1000.000000000000000 ) ;
#7025 = CARTESIAN_POINT ( 'NONE',  ( -174.7846310273254176, 131.4932641812416421, 2.500000000270498735 ) ) ;
#7026 = CARTESIAN_POINT ( 'NONE',  ( 0.1708300674639733063, -1.717253364505205271, 2.525629923208374539 ) ) ;
#7027 = DIRECTION ( 'NONE',  ( 0.000000000000000000, 0.9902680687415714722, -0.1391731009600582769 ) ) ;
#7028 = AXIS2_PLACEMENT_3D ( 'NONE', #6811, #3405, #1029 ) ;
#7029 = VERTEX_POINT ( 'NONE', #14487 ) ;
#7030 = AXIS2_PLACEMENT_3D ( 'NONE', #15033, #9060, #6464 ) ;
#7031 = ORIENTED_EDGE ( 'NONE', *, *, #4301, .F. ) ;
#7032 = DIRECTION ( 'NONE',  ( -1.000000000000000000, 0.000000000000000000, 0.000000000000000000 ) ) ;
#7033 = CARTESIAN_POINT ( 'NONE',  ( -76.50000000000002842, 19.53993994372674337, 9.999999999999998224 ) ) ;
#7034 = CARTESIAN_POINT ( 'NONE',  ( 0.3167204509598386397, -8.479269695850858213, 1.313474075707245392 ) ) ;
#7035 = CARTESIAN_POINT ( 'NONE',  ( 14.00000000000004086, 64.51493994372674479, 15.00000000000104983 ) ) ;
#7036 = FACE_OUTER_BOUND ( 'NONE', #10597, .T. ) ;
#7037 = ADVANCED_FACE ( 'NONE', ( #12052 ), #7412, .F. ) ;
#7038 = ADVANCED_FACE ( 'NONE', ( #11030 ), #8845, .T. ) ;
#7039 = EDGE_LOOP ( 'NONE', ( #10795, #10834 ) ) ;
#7040 = AXIS2_PLACEMENT_3D ( 'NONE', #12117, #5170, #3598 ) ;
#7041 = SHAPE_REPRESENTATION ( 'Long Manual Lever Operating Handle', ( #12337 ), #6268 ) ;
#7042 = ORIENTED_EDGE ( 'NONE', *, *, #8760, .T. ) ;
#7043 = CARTESIAN_POINT ( 'NONE',  ( 172.5293059057019889, 61.25683321636181233, 9.975000000000001421 ) ) ;
#7044 = EDGE_LOOP ( 'NONE', ( #11648, #6838 ) ) ;
#7045 = CARTESIAN_POINT ( 'NONE',  ( 14.00000000000004086, 59.53993994372674337, 13.30000000000105231 ) ) ;
#7046 = CARTESIAN_POINT ( 'NONE',  ( -225.6712625649270478, 142.9137214952622514, 1.583163137451349511 ) ) ;
#7047 = ORIENTED_EDGE ( 'NONE', *, *, #7803, .F. ) ;
#7048 = ORIENTED_EDGE ( 'NONE', *, *, #1028, .F. ) ;
#7049 = DIRECTION ( 'NONE',  ( 1.000000000000000000, 0.000000000000000000, 0.000000000000000000 ) ) ;
#7050 = CARTESIAN_POINT ( 'NONE',  ( 200.1062858801516597, 33.86394065090269123, 10.00000000000000533 ) ) ;
#7051 = AXIS2_PLACEMENT_3D ( 'NONE', #9024, #7690, #9980 ) ;
#7052 = ADVANCED_FACE ( 'NONE', ( #342 ), #11352, .F. ) ;
#7053 = ORIENTED_EDGE ( 'NONE', *, *, #1398, .F. ) ;
#7054 = CARTESIAN_POINT ( 'NONE',  ( -222.0995690897443922, 149.3129710173510887, 2.431557144026069928 ) ) ;
#7055 = CARTESIAN_POINT ( 'NONE',  ( 5.799999999999999822, 9.237604307034018802, 0.000000000000000000 ) ) ;
#7056 = DIRECTION ( 'NONE',  ( 0.9296197478520976665, 0.3660421972118349521, -0.04266420354037676888 ) ) ;
#7057 = AXIS2_PLACEMENT_3D ( 'NONE', #1055, #5880, #10698 ) ;
#7058 = AXIS2_PLACEMENT_3D ( 'NONE', #14307, #3506, #6039 ) ;
#7059 = AXIS2_PLACEMENT_3D ( 'NONE', #6504, #11304, #14923 ) ;
#7060 = ORIENTED_EDGE ( 'NONE', *, *, #3199, .F. ) ;
#7061 = CARTESIAN_POINT ( 'NONE',  ( -64.00000000000002842, 16.03993994372673981, 38.07518420361041933 ) ) ;
#7062 =( REPRESENTATION_RELATIONSHIP ('NONE','NONE', #3298, #11876 ) REPRESENTATION_RELATIONSHIP_WITH_TRANSFORMATION ( #2445 )SHAPE_REPRESENTATION_RELATIONSHIP( ) );
#7063 = ORIENTED_EDGE ( 'NONE', *, *, #7583, .F. ) ;
#7064 = LINE ( 'NONE', #11872, #6948 ) ;
#7065 = CARTESIAN_POINT ( 'NONE',  ( 177.5000000000000853, 15.53993994372673804, 24.94742576086838781 ) ) ;
#7066 = DIRECTION ( 'NONE',  ( -0.000000000000000000, -0.000000000000000000, 1.000000000000000000 ) ) ;
#7067 = AXIS2_PLACEMENT_3D ( 'NONE', #10320, #8987, #7729 ) ;
#7068 = ORIENTED_EDGE ( 'NONE', *, *, #10427, .T. ) ;
#7069 = CARTESIAN_POINT ( 'NONE',  ( -212.3935931674892856, 139.5852744332111683, -4.642206099735020963 ) ) ;
#7070 = CARTESIAN_POINT ( 'NONE',  ( 207.3736904795575811, 50.31851200600168994, -2.642755332960478043 ) ) ;
#7071 = ORIENTED_EDGE ( 'NONE', *, *, #5856, .T. ) ;
#7072 = VECTOR ( 'NONE', #4969, 1000.000000000000000 ) ;
#7073 = EDGE_CURVE ( 'NONE', #14472, #9526, #14622, .T. ) ;
#7074 = AXIS2_PLACEMENT_3D ( 'NONE', #6903, #10369, #8097 ) ;
#7075 = DIRECTION ( 'NONE',  ( 0.000000000000000000, 0.000000000000000000, -1.000000000000000000 ) ) ;
#7076 = CARTESIAN_POINT ( 'NONE',  ( -63.50000000000002842, 19.53993994372674692, -17.50000000000002487 ) ) ;
#7077 = CARTESIAN_POINT ( 'NONE',  ( -152.0205871941159614, 106.4705699334293598, -4.325135862343421955 ) ) ;
#7078 = VECTOR ( 'NONE', #13830, 1000.000000000000000 ) ;
#7079 = ORIENTED_EDGE ( 'NONE', *, *, #4595, .T. ) ;
#7080 = AXIS2_PLACEMENT_3D ( 'NONE', #15119, #832, #9152 ) ;
#7081 = AXIS2_PLACEMENT_3D ( 'NONE', #11113, #266, #13387 ) ;
#7082 = CARTESIAN_POINT ( 'NONE',  ( 207.1663125311009992, 46.09156421935289671, -5.616260741029326375 ) ) ;
#7083 = B_SPLINE_CURVE_WITH_KNOTS ( 'NONE', 3,
 ( #3335, #6977, #11862, #4667, #1036, #11939, #12954, #5862, #9494, #14290, #3483, #2302, #2618, #7597, #9652, #13338 ),
 .UNSPECIFIED., .F., .F.,
 ( 4, 2, 2, 2, 2, 2, 2, 4 ),
 ( 0.000000000000000000, 0.0004036473355434109611, 0.0008072946710868219222, 0.001210942006630233046, 0.001614589342173643844, 0.002421884013260385427, 0.002825531348803770638, 0.003229178684347154982 ),
 .UNSPECIFIED. ) ;
#7084 = VERTEX_POINT ( 'NONE', #5335 ) ;
#7085 = CARTESIAN_POINT ( 'NONE',  ( -223.5244451892836537, 142.1828519274101836, 0.6844914428394093253 ) ) ;
#7086 = CARTESIAN_POINT ( 'NONE',  ( -209.4369489341841586, 132.9646294043573675, 1.515400478619103763 ) ) ;
#7087 = DIRECTION ( 'NONE',  ( 0.4630766004634062072, 0.8863182623094566503, 0.000000000000000000 ) ) ;
#7088 = CARTESIAN_POINT ( 'NONE',  ( 190.5000000000000568, 15.17911304468679923, 9.062306170389897275 ) ) ;
#7089 = LINE ( 'NONE', #3755, #506 ) ;
#7090 = ORIENTED_EDGE ( 'NONE', *, *, #164, .F. ) ;
#7091 = ORIENTED_EDGE ( 'NONE', *, *, #7158, .F. ) ;
#7092 = DIRECTION ( 'NONE',  ( 1.000000000000000000, -0.000000000000000000, -0.000000000000000000 ) ) ;
#7093 = DIRECTION ( 'NONE',  ( 0.000000000000000000, 0.000000000000000000, -1.000000000000000000 ) ) ;
#7094 = EDGE_CURVE ( 'NONE', #6265, #10437, #10234, .T. ) ;
#7095 = VECTOR ( 'NONE', #10018, 1000.000000000000000 ) ;
#7096 = DIRECTION ( 'NONE',  ( -1.000000000000000000, 0.000000000000000000, 0.000000000000000000 ) ) ;
#7097 = FACE_OUTER_BOUND ( 'NONE', #7264, .T. ) ;
#7098 = CARTESIAN_POINT ( 'NONE',  ( -224.1994838851412624, 145.5506440303793454, -0.5027386706791425741 ) ) ;
#7099 = CARTESIAN_POINT ( 'NONE',  ( -218.7472433255651936, 151.2978141277262409, 9.195915456466519089 ) ) ;
#7100 = CARTESIAN_POINT ( 'NONE',  ( -1.014660767515926061E-14, -0.7818963812181285444, -7.999999999999981348 ) ) ;
#7101 = ADVANCED_FACE ( 'NONE', ( #7880 ), #12358, .T. ) ;
#7102 = CIRCLE ( 'NONE', #8610, 5.000000000000004441 ) ;
#7103 = DIRECTION ( 'NONE',  ( 1.000000000000000000, 0.000000000000000000, 0.000000000000000000 ) ) ;
#7104 = CARTESIAN_POINT ( 'NONE',  ( 178.0000000000000853, -178.8753867012115961, -29.82329228561640022 ) ) ;
#7105 = AXIS2_PLACEMENT_3D ( 'NONE', #5092, #3514, #8351 ) ;
#7106 = DIRECTION ( 'NONE',  ( -1.000000000000000000, 0.000000000000000000, 0.000000000000000000 ) ) ;
#7107 = ORIENTED_EDGE ( 'NONE', *, *, #2859, .F. ) ;
#7108 = EDGE_CURVE ( 'NONE', #11153, #14187, #2277, .T. ) ;
#7109 =( NAMED_UNIT ( * ) PLANE_ANGLE_UNIT ( ) SI_UNIT ( $, .RADIAN. ) );
#7110 = ORIENTED_EDGE ( 'NONE', *, *, #2606, .T. ) ;
#7111 = DIRECTION ( 'NONE',  ( 1.000000000000000000, 0.000000000000000000, 0.000000000000000000 ) ) ;
#7112 = DIRECTION ( 'NONE',  ( 0.000000000000000000, 0.000000000000000000, -1.000000000000000000 ) ) ;
#7113 =( NAMED_UNIT ( * ) PLANE_ANGLE_UNIT ( ) SI_UNIT ( $, .RADIAN. ) );
#7114 = LINE ( 'NONE', #12775, #565 ) ;
#7115 = DIRECTION ( 'NONE',  ( -1.000000000000000000, 0.000000000000000000, -0.000000000000000000 ) ) ;
#7116 = EDGE_CURVE ( 'NONE', #6706, #2958, #5182, .T. ) ;
#7117 = CIRCLE ( 'NONE', #5599, 1.699999999999993072 ) ;
#7118 = CARTESIAN_POINT ( 'NONE',  ( -211.2987210398670186, 151.8733316563206586, 2.500000000000000000 ) ) ;
#7119 = AXIS2_PLACEMENT_3D ( 'NONE', #1085, #10651, #9389 ) ;
#7120 = ORIENTED_EDGE ( 'NONE', *, *, #13360, .F. ) ;
#7121 = ORIENTED_EDGE ( 'NONE', *, *, #9816, .T. ) ;
#7122 = CARTESIAN_POINT ( 'NONE',  ( 207.1131222881253393, 35.56952893079440514, -7.807171136772324438 ) ) ;
#7123 = FACE_OUTER_BOUND ( 'NONE', #9277, .T. ) ;
#7124 = ORIENTED_EDGE ( 'NONE', *, *, #7965, .F. ) ;
#7125 = CARTESIAN_POINT ( 'NONE',  ( -85.99999999999994316, 62.13993994372673768, 15.00000000000174794 ) ) ;
#7126 = AXIS2_PLACEMENT_3D ( 'NONE', #3696, #5120, #7349 ) ;
#7127 = ADVANCED_FACE ( 'NONE', ( #13533 ), #6692, .F. ) ;
#7128 = ADVANCED_FACE ( 'NONE', ( #414 ), #8902, .F. ) ;
#7129 = ADVANCED_FACE ( 'NONE', ( #4141, #1544 ), #6380, .T. ) ;
#7130 = CARTESIAN_POINT ( 'NONE',  ( -224.5263272834600059, 144.9650527765320192, 3.765861206744722356 ) ) ;
#7131 = EDGE_LOOP ( 'NONE', ( #337, #11198, #11234, #3434 ) ) ;
#7132 = VERTEX_POINT ( 'NONE', #5496 ) ;
#7133 = CARTESIAN_POINT ( 'NONE',  ( -10.39230484541326582, 4.570335331080236228E-16, 5.000000000000000000 ) ) ;
#7134 = CARTESIAN_POINT ( 'NONE',  ( 0.000000000000000000, 0.000000000000000000, 0.000000000000000000 ) ) ;
#7135 = EDGE_LOOP ( 'NONE', ( #3925, #10122, #11133, #7491 ) ) ;
#7136 = CARTESIAN_POINT ( 'NONE',  ( 64.00000000000005684, 59.53993994372674337, 15.00000000000070166 ) ) ;
#7137 = CARTESIAN_POINT ( 'NONE',  ( -86.97455057502459397, 65.19100426474074084, 7.600000000000002309 ) ) ;
#7138 = CIRCLE ( 'NONE', #5865, 0.5000000000000001110 ) ;
#7139 = EDGE_CURVE ( 'NONE', #470, #3955, #11866, .T. ) ;
#7140 = ORIENTED_EDGE ( 'NONE', *, *, #6842, .F. ) ;
#7141 = DIRECTION ( 'NONE',  ( -1.000000000000000000, 0.000000000000000000, 0.000000000000000000 ) ) ;
#7142 = DIRECTION ( 'NONE',  ( -1.000000000000000000, 0.000000000000000000, -0.000000000000000000 ) ) ;
#7143 = ORIENTED_EDGE ( 'NONE', *, *, #1114, .F. ) ;
#7144 = CARTESIAN_POINT ( 'NONE',  ( -85.27455057502459113, 65.19100426474074084, 10.00000000000000178 ) ) ;
#7145 = CARTESIAN_POINT ( 'NONE',  ( -177.3557003870508595, 132.9282874014947140, 2.500000000000000000 ) ) ;
#7146 = CYLINDRICAL_SURFACE ( 'NONE', #3507, 1.499999999999994449 ) ;
#7147 = EDGE_LOOP ( 'NONE', ( #589, #12930, #9019, #5070 ) ) ;
#7148 = ORIENTED_EDGE ( 'NONE', *, *, #13825, .F. ) ;
#7149 = CARTESIAN_POINT ( 'NONE',  ( -206.8675068987516283, 149.4103724542255804, 1.515441477536285220 ) ) ;
#7150 = CARTESIAN_POINT ( 'NONE',  ( 193.0579178353149246, 46.09544038230585272, -7.876361695281355324 ) ) ;
#7151 = ORIENTED_EDGE ( 'NONE', *, *, #4463, .F. ) ;
#7152 = AXIS2_PLACEMENT_3D ( 'NONE', #4415, #14043, #3234 ) ;
#7153 = CARTESIAN_POINT ( 'NONE',  ( -10.39230484541326582, 4.570335331080236228E-16, 0.000000000000000000 ) ) ;
#7154 = DIRECTION ( 'NONE',  ( 0.000000000000000000, -0.000000000000000000, -1.000000000000000000 ) ) ;
#7155 = DIRECTION ( 'NONE',  ( 0.000000000000000000, 0.000000000000000000, -1.000000000000000000 ) ) ;
#7156 = VECTOR ( 'NONE', #14891, 1000.000000000000000 ) ;
#7157 = EDGE_CURVE ( 'NONE', #3263, #1447, #14791, .T. ) ;
#7158 = EDGE_CURVE ( 'NONE', #10500, #14360, #581, .T. ) ;
#7159 = ORIENTED_EDGE ( 'NONE', *, *, #5828, .T. ) ;
#7160 = ADVANCED_FACE ( 'NONE', ( #6615 ), #2796, .T. ) ;
#7161 = DIRECTION ( 'NONE',  ( 0.5609955855128418989, 0.8160197353768049444, 0.1392686056176078435 ) ) ;
#7162 = CARTESIAN_POINT ( 'NONE',  ( 126.0806775638430253, 45.00321902537314145, 10.00000000000000178 ) ) ;
#7163 = CARTESIAN_POINT ( 'NONE',  ( 194.7957337413261030, 33.86335648926068842, -5.558215102112974648 ) ) ;
#7164 = EDGE_LOOP ( 'NONE', ( #15135, #6549, #1192 ) ) ;
#7165 = CARTESIAN_POINT ( 'NONE',  ( 15.71029453487719074, 40.04259805664093363, 10.00000000000000178 ) ) ;
#7166 = DIRECTION ( 'NONE',  ( -0.000000000000000000, -0.000000000000000000, -1.000000000000000000 ) ) ;
#7167 = AXIS2_PLACEMENT_3D ( 'NONE', #759, #10412, #10561 ) ;
#7168 = CARTESIAN_POINT ( 'NONE',  ( -225.5658467874630446, 143.1025904080742919, 5.367833425961707761 ) ) ;
#7169 = CARTESIAN_POINT ( 'NONE',  ( 66.76535645333922275, 38.79159067395544014, 9.975000000000001421 ) ) ;
#7170 = CARTESIAN_POINT ( 'NONE',  ( -152.4086188282879277, 107.2728346664360259, 9.411501811869209533 ) ) ;
#7171 = CARTESIAN_POINT ( 'NONE',  ( -216.0863581598438543, 143.0557482234525253, 9.577123744044239828 ) ) ;
#7172 = DIRECTION ( 'NONE',  ( -3.965082230804130220E-16, 0.000000000000000000, 1.000000000000000000 ) ) ;
#7173 = AXIS2_PLACEMENT_3D ( 'NONE', #7479, #1226, #4708 ) ;
#7174 = EDGE_LOOP ( 'NONE', ( #3580, #6115, #9982, #10506, #10000 ) ) ;
#7175 = VERTEX_POINT ( 'NONE', #13613 ) ;
#7176 = FACE_OUTER_BOUND ( 'NONE', #4866, .T. ) ;
#7177 = CYLINDRICAL_SURFACE ( 'NONE', #4790, 1.500000000000001332 ) ;
#7178 = FACE_OUTER_BOUND ( 'NONE', #7407, .T. ) ;
#7179 = DIRECTION ( 'NONE',  ( 0.000000000000000000, -0.1391731009600582492, -0.9902680687415713612 ) ) ;
#7180 = EDGE_CURVE ( 'NONE', #8016, #10578, #11616, .T. ) ;
#7181 = DIRECTION ( 'NONE',  ( 0.000000000000000000, 0.000000000000000000, -1.000000000000000000 ) ) ;
#7182 = AXIS2_PLACEMENT_3D ( 'NONE', #5032, #183, #3767 ) ;
#7183 = EDGE_CURVE ( 'NONE', #12077, #11157, #496, .T. ) ;
#7184 = CARTESIAN_POINT ( 'NONE',  ( -221.9362923240670114, 145.3446861235061931, 9.019126511735166218 ) ) ;
#7185 = AXIS2_PLACEMENT_3D ( 'NONE', #912, #10557, #1941 ) ;
#7186 = CARTESIAN_POINT ( 'NONE',  ( -85.99999999999994316, 59.53993994372674337, 15.00000000000174794 ) ) ;
#7187 = CARTESIAN_POINT ( 'NONE',  ( 0.000000000000000000, 9.237604307034018802, 0.000000000000000000 ) ) ;
#7188 = CARTESIAN_POINT ( 'NONE',  ( -64.00000000000002842, 13.40307322461931072, 37.29540324609171620 ) ) ;
#7189 = DIRECTION ( 'NONE',  ( -0.000000000000000000, -0.000000000000000000, 1.000000000000000000 ) ) ;
#7190 = FACE_OUTER_BOUND ( 'NONE', #7283, .T. ) ;
#7191 = FACE_BOUND ( 'NONE', #2907, .T. ) ;
#7192 = ORIENTED_EDGE ( 'NONE', *, *, #318, .T. ) ;
#7193 = ADVANCED_FACE ( 'NONE', ( #11262 ), #8027, .F. ) ;
#7194 = AXIS2_PLACEMENT_3D ( 'NONE', #2193, #2035, #15359 ) ;
#7195 = ORIENTED_EDGE ( 'NONE', *, *, #9811, .T. ) ;
#7196 = FACE_OUTER_BOUND ( 'NONE', #3599, .T. ) ;
#7197 = DIRECTION ( 'NONE',  ( 0.8731965799097684000, -0.4873681696970815769, -0.000000000000000000 ) ) ;
#7198 = FACE_OUTER_BOUND ( 'NONE', #12216, .T. ) ;
#7199 = FILL_AREA_STYLE ('',( #2361 ) ) ;
#7200 = CARTESIAN_POINT ( 'NONE',  ( 177.5000000000000853, 16.03993994372673981, -17.50000000000002487 ) ) ;
#7201 = DIRECTION ( 'NONE',  ( -0.000000000000000000, -0.000000000000000000, -1.000000000000000000 ) ) ;
#7202 = DIRECTION ( 'NONE',  ( 0.000000000000000000, 0.000000000000000000, 1.000000000000000000 ) ) ;
#7203 = VERTEX_POINT ( 'NONE', #15181 ) ;
#7204 = EDGE_CURVE ( 'NONE', #9977, #11227, #11366, .T. ) ;
#7205 = VERTEX_POINT ( 'NONE', #3278 ) ;
#7206 = CARTESIAN_POINT ( 'NONE',  ( 208.8186272397570349, 39.68461847005694665, -7.558035125831273682 ) ) ;
#7207 = DIRECTION ( 'NONE',  ( 0.000000000000000000, -1.000000000000000000, 0.000000000000000000 ) ) ;
#7208 = ORIENTED_EDGE ( 'NONE', *, *, #765, .F. ) ;
#7209 = CARTESIAN_POINT ( 'NONE',  ( -222.1550322922110752, 144.9192006534358370, 8.707947314692312091 ) ) ;
#7210 = ORIENTED_EDGE ( 'NONE', *, *, #3469, .F. ) ;
#7211 = EDGE_LOOP ( 'NONE', ( #12829, #14920, #8765, #13726 ) ) ;
#7212 = DIRECTION ( 'NONE',  ( 0.000000000000000000, 0.000000000000000000, -1.000000000000000000 ) ) ;
#7213 = CARTESIAN_POINT ( 'NONE',  ( 64.00000000000005684, 64.51493994372674479, 15.00000000000070166 ) ) ;
#7214 = ORIENTED_EDGE ( 'NONE', *, *, #11456, .T. ) ;
#7215 = DIRECTION ( 'NONE',  ( 1.000000000000000000, 0.000000000000000000, 0.000000000000000000 ) ) ;
#7216 = DIRECTION ( 'NONE',  ( 0.000000000000000000, -0.000000000000000000, 1.000000000000000000 ) ) ;
#7217 = EDGE_CURVE ( 'NONE', #2296, #4912, #8107, .T. ) ;
#7219 = EDGE_CURVE ( 'NONE', #7650, #9167, #814, .T. ) ;
#7218 = EDGE_CURVE ( 'NONE', #10763, #13859, #3299, .T. ) ;
#7220 = VECTOR ( 'NONE', #8869, 1000.000000000000114 ) ;
#7221 = ORIENTED_EDGE ( 'NONE', *, *, #11318, .T. ) ;
#7222 =( NAMED_UNIT ( * ) PLANE_ANGLE_UNIT ( ) SI_UNIT ( $, .RADIAN. ) );
#7223 = EDGE_CURVE ( 'NONE', #2412, #10382, #7346, .T. ) ;
#7224 = ORIENTED_EDGE ( 'NONE', *, *, #13117, .T. ) ;
#7225 = VECTOR ( 'NONE', #1200, 1000.000000000000114 ) ;
#7226 = CYLINDRICAL_SURFACE ( 'NONE', #2920, 0.5000000000000004441 ) ;
#7227 = DIRECTION ( 'NONE',  ( -0.7071067811865500152, 0.000000000000000000, 0.7071067811865451302 ) ) ;
#7228 = DIRECTION ( 'NONE',  ( -0.8731965799097685110, 0.4873681696970816324, 0.000000000000000000 ) ) ;
#7229 = ORIENTED_EDGE ( 'NONE', *, *, #6028, .T. ) ;
#7230 = ORIENTED_EDGE ( 'NONE', *, *, #5370, .F. ) ;
#7231 = CARTESIAN_POINT ( 'NONE',  ( -192.1661132380199604, 141.2048990416207630, 1.515441477536284332 ) ) ;
#7232 = CARTESIAN_POINT ( 'NONE',  ( 211.8867585259220050, 39.31811064754020890, -6.135149402309513000 ) ) ;
#7233 = ORIENTED_EDGE ( 'NONE', *, *, #3867, .F. ) ;
#7234 = DIRECTION ( 'NONE',  ( -0.000000000000000000, -0.000000000000000000, 1.000000000000000000 ) ) ;
#7235 = CARTESIAN_POINT ( 'NONE',  ( -130.0135953313997561, 106.9229804370480537, 0.000000000000000000 ) ) ;
#7236 = CARTESIAN_POINT ( 'NONE',  ( 177.5000000000000853, -178.6666270497714777, -18.18093594598675011 ) ) ;
#7237 = AXIS2_PLACEMENT_3D ( 'NONE', #12274, #6292, #9855 ) ;
#7238 = ORIENTED_EDGE ( 'NONE', *, *, #13234, .F. ) ;
#7239 = SURFACE_SIDE_STYLE ('',( #897 ) ) ;
#7240 = CARTESIAN_POINT ( 'NONE',  ( 208.8162124854775357, 42.04914431719598156, -1.433821094984975009 ) ) ;
#7241 = EDGE_LOOP ( 'NONE', ( #5173, #2181, #5548, #9764 ) ) ;
#7242 = DIRECTION ( 'NONE',  ( -0.000000000000000000, -0.000000000000000000, -1.000000000000000000 ) ) ;
#7243 = DIRECTION ( 'NONE',  ( -0.000000000000000000, -8.673617379884035472E-17, 1.000000000000000000 ) ) ;
#7244 = EDGE_CURVE ( 'NONE', #5951, #10303, #13836, .T. ) ;
#7245 = CARTESIAN_POINT ( 'NONE',  ( -187.5349220100912930, 120.9938564418671518, 1.515400478619096658 ) ) ;
#7246 = CARTESIAN_POINT ( 'NONE',  ( 200.1062858801516597, 40.86394065090267702, 5.000000000000000000 ) ) ;
#7247 = ORIENTED_EDGE ( 'NONE', *, *, #8923, .F. ) ;
#7248 = CARTESIAN_POINT ( 'NONE',  ( -169.4720549176639395, 123.8986143635366943, 9.496311331651778431 ) ) ;
#7249 = CARTESIAN_POINT ( 'NONE',  ( 194.0000000000000568, 59.53993994372674337, 20.00000000000000355 ) ) ;
#7250 = ORIENTED_EDGE ( 'NONE', *, *, #8363, .F. ) ;
#7251 = ORIENTED_EDGE ( 'NONE', *, *, #10593, .F. ) ;
#7252 = DIRECTION ( 'NONE',  ( 1.000000000000000000, 0.000000000000000000, 0.000000000000000000 ) ) ;
#7253 = DIRECTION ( 'NONE',  ( 0.000000000000000000, 0.000000000000000000, 1.000000000000000000 ) ) ;
#7254 = EDGE_CURVE ( 'NONE', #815, #4028, #11570, .T. ) ;
#7255 = CARTESIAN_POINT ( 'NONE',  ( 178.0000000000000853, 15.53993994372673804, 24.94742576086838781 ) ) ;
#7256 = FACE_OUTER_BOUND ( 'NONE', #7950, .T. ) ;
#7257 = DIRECTION ( 'NONE',  ( 0.000000000000000000, 0.000000000000000000, 1.000000000000000000 ) ) ;
#7258 = CARTESIAN_POINT ( 'NONE',  ( -217.3694051724266671, 153.7302547217275333, 6.764857390201539644 ) ) ;
#7259 = CARTESIAN_POINT ( 'NONE',  ( 164.0000000000000568, 62.13993994372673768, 13.29999999999999538 ) ) ;
#7260 = CARTESIAN_POINT ( 'NONE',  ( -155.6477983077462852, 110.0653742669871917, 9.691934182417337951 ) ) ;
#7261 = DIRECTION ( 'NONE',  ( 1.000000000000000000, 0.000000000000000000, 0.000000000000000000 ) ) ;
#7262 = FACE_BOUND ( 'NONE', #8493, .T. ) ;
#7263 = DIRECTION ( 'NONE',  ( -1.000000000000000000, -0.000000000000000000, -0.000000000000000000 ) ) ;
#7264 = EDGE_LOOP ( 'NONE', ( #4870, #89, #12730, #14315 ) ) ;
#7265 = ORIENTED_EDGE ( 'NONE', *, *, #10773, .F. ) ;
#7266 = ADVANCED_FACE ( 'NONE', ( #3432, #12818 ), #14080, .T. ) ;
#7267 = DIRECTION ( 'NONE',  ( 1.000000000000000000, 0.000000000000000000, 0.000000000000000000 ) ) ;
#7268 = CARTESIAN_POINT ( 'NONE',  ( -64.00000000000002842, -178.7362136002515172, 52.68580191161573367 ) ) ;
#7269 = CARTESIAN_POINT ( 'NONE',  ( -88.77455057502459113, 65.19100426474074084, 9.975000000000001421 ) ) ;
#7270 = FACE_OUTER_BOUND ( 'NONE', #7402, .T. ) ;
#7271 = CARTESIAN_POINT ( 'NONE',  ( 0.1714848819421568860, 1.330901335693120302, 2.750000000000000888 ) ) ;
#7272 = CARTESIAN_POINT ( 'NONE',  ( 200.1062858801516597, 40.86394065090267702, 0.000000000000000000 ) ) ;
#7273 = DIRECTION ( 'NONE',  ( 0.000000000000000000, -1.000000000000000000, 0.000000000000000000 ) ) ;
#7274 =( REPRESENTATION_RELATIONSHIP ('NONE','NONE', #3298, #13652 ) REPRESENTATION_RELATIONSHIP_WITH_TRANSFORMATION ( #4341 )SHAPE_REPRESENTATION_RELATIONSHIP( ) );
#7275 = VERTEX_POINT ( 'NONE', #10621 ) ;
#7276 = AXIS2_PLACEMENT_3D ( 'NONE', #12602, #1865, #3068 ) ;
#7277 = AXIS2_PLACEMENT_3D ( 'NONE', #4752, #15548, #7142 ) ;
#7278 = ORIENTED_EDGE ( 'NONE', *, *, #9098, .F. ) ;
#7279 = CARTESIAN_POINT ( 'NONE',  ( 201.9353358396146234, 32.56853033914327966, -9.715529407007519325 ) ) ;
#7280 = SURFACE_SIDE_STYLE ('',( #10746 ) ) ;
#7281 = ORIENTED_EDGE ( 'NONE', *, *, #14175, .F. ) ;
#7282 = CARTESIAN_POINT ( 'NONE',  ( -223.3638075659000606, 147.0478893353539718, 7.150006577359191873 ) ) ;
#7283 = EDGE_LOOP ( 'NONE', ( #12532, #7214, #767, #8210 ) ) ;
#7284 = ORIENTED_EDGE ( 'NONE', *, *, #8741, .F. ) ;
#7285 = CARTESIAN_POINT ( 'NONE',  ( 175.9483885134608272, -178.8058001507315566, 52.69066787724494816 ) ) ;
#7286 = DIRECTION ( 'NONE',  ( 0.000000000000000000, 0.000000000000000000, -1.000000000000000000 ) ) ;
#7287 = ADVANCED_FACE ( 'NONE', ( #11729 ), #7557, .T. ) ;
#7288 = VERTEX_POINT ( 'NONE', #4613 ) ;
#7289 = CIRCLE ( 'NONE', #9296, 1.700000000000000178 ) ;
#7290 = CARTESIAN_POINT ( 'NONE',  ( -76.50000000000004263, -179.8058001507315566, 52.19066787724494816 ) ) ;
#7291 = CYLINDRICAL_SURFACE ( 'NONE', #8093, 3.500000000000003109 ) ;
#7292 = CARTESIAN_POINT ( 'NONE',  ( -76.50000000000004263, 16.03993994372673626, 37.49999999999991473 ) ) ;
#7293 = CIRCLE ( 'NONE', #441, 4.499999999999950262 ) ;
#7294 = CARTESIAN_POINT ( 'NONE',  ( 5.799999999999999822, -4.618802153517037823, -7.999999999999979572 ) ) ;
#7295 = EDGE_LOOP ( 'NONE', ( #10877, #7305 ) ) ;
#7296 = CARTESIAN_POINT ( 'NONE',  ( -70.00000000000000000, -201.3058001507315566, -41.45141194869120227 ) ) ;
#7297 = EDGE_CURVE ( 'NONE', #3756, #12140, #10063, .T. ) ;
#7299 = AXIS2_PLACEMENT_3D ( 'NONE', #13442, #2640, #3589 ) ;
#7298 = DIRECTION ( 'NONE',  ( 0.000000000000000000, 0.000000000000000000, -1.000000000000000000 ) ) ;
#7300 = CARTESIAN_POINT ( 'NONE',  ( 177.5000000000000853, 16.03993994372673626, 38.07518420361041933 ) ) ;
#7301 = VERTEX_POINT ( 'NONE', #14160 ) ;
#7302 = VERTEX_POINT ( 'NONE', #8265 ) ;
#7303 = CARTESIAN_POINT ( 'NONE',  ( -200.7948432279144129, 140.6912097071583787, -4.640918829492429509 ) ) ;
#7304 = CARTESIAN_POINT ( 'NONE',  ( 207.1592428330643827, 35.64176030267155681, -3.375779224823745928 ) ) ;
#7305 = ORIENTED_EDGE ( 'NONE', *, *, #7204, .F. ) ;
#7306 = PRODUCT_RELATED_PRODUCT_CATEGORY ( 'part', '', ( #8040 ) ) ;
#7307 = CARTESIAN_POINT ( 'NONE',  ( 13.07968152355895874, 460.3807876674321165, 0.000000000000000000 ) ) ;
#7308 = CARTESIAN_POINT ( 'NONE',  ( -108.0000000000000568, 64.53993994372673626, 10.00000000000000178 ) ) ;
#7309 = AXIS2_PLACEMENT_3D ( 'NONE', #6356, #2954, #7773 ) ;
#7310 = EDGE_CURVE ( 'NONE', #3093, #6329, #11205, .T. ) ;
#7311 = CYLINDRICAL_SURFACE ( 'NONE', #9323, 1.700000000000000178 ) ;
#7312 = VECTOR ( 'NONE', #9505, 1000.000000000000000 ) ;
#7313 = ORIENTED_EDGE ( 'NONE', *, *, #12226, .F. ) ;
#7314 = SURFACE_STYLE_FILL_AREA ( #6278 ) ;
#7315 = AXIS2_PLACEMENT_3D ( 'NONE', #4223, #7809, #2978 ) ;
#7316 = CARTESIAN_POINT ( 'NONE',  ( 211.9048830940805885, 42.38452776791458376, -2.873977808594950112 ) ) ;
#7317 = EDGE_LOOP ( 'NONE', ( #6428, #2721, #6389 ) ) ;
#7318 = CARTESIAN_POINT ( 'NONE',  ( 190.0000000000001137, -178.8058001507315566, 65.31842631998698323 ) ) ;
#7319 = DIRECTION ( 'NONE',  ( 0.000000000000000000, 1.734723475976805517E-15, 1.000000000000000000 ) ) ;
#7320 = CARTESIAN_POINT ( 'NONE',  ( -182.0950013669840359, 118.3955881831737997, 1.446957622915671537 ) ) ;
#7321 = AXIS2_PLACEMENT_3D ( 'NONE', #11433, #13878, #434 ) ;
#7322 = CARTESIAN_POINT ( 'NONE',  ( -76.50000000000001421, 17.53993994372673981, -17.50000000000002487 ) ) ;
#7323 = ORIENTED_EDGE ( 'NONE', *, *, #14726, .F. ) ;
#7324 = CARTESIAN_POINT ( 'NONE',  ( -173.3126422121597443, 122.7186289792270912, 10.06128868882609062 ) ) ;
#7325 = DIRECTION ( 'NONE',  ( 1.000000000000000000, 0.000000000000000000, 0.000000000000000000 ) ) ;
#7326 = ADVANCED_FACE ( 'NONE', ( #14007, #10387 ), #5882, .F. ) ;
#7327 = ORIENTED_EDGE ( 'NONE', *, *, #3721, .T. ) ;
#7328 = EDGE_CURVE ( 'NONE', #12014, #8771, #7392, .T. ) ;
#7329 = ORIENTED_EDGE ( 'NONE', *, *, #2190, .T. ) ;
#7330 = CARTESIAN_POINT ( 'NONE',  ( 190.5000000000000568, 17.53993994372674692, -17.50000000000002487 ) ) ;
#7331 = CARTESIAN_POINT ( 'NONE',  ( 64.00000000000005684, 64.53993994372673626, 15.00000000000070166 ) ) ;
#7332 = FACE_OUTER_BOUND ( 'NONE', #5782, .T. ) ;
#7333 = LINE ( 'NONE', #1307, #4957 ) ;
#7334 = AXIS2_PLACEMENT_3D ( 'NONE', #11784, #951, #15394 ) ;
#7335 = DIRECTION ( 'NONE',  ( 0.000000000000000000, 1.000000000000000000, 0.000000000000000000 ) ) ;
#7336 = CIRCLE ( 'NONE', #495, 0.5000000000000004441 ) ;
#7337 = VECTOR ( 'NONE', #4877, 1000.000000000000000 ) ;
#7338 = CARTESIAN_POINT ( 'NONE',  ( 0.000000000000000000, -2.775557561562891351E-14, -8.000000000000007105 ) ) ;
#7339 = DIRECTION ( 'NONE',  ( 0.000000000000000000, -0.1391731009600592484, -0.9902680687415712502 ) ) ;
#7340 = EDGE_CURVE ( 'NONE', #7302, #12019, #3826, .T. ) ;
#7341 = DIRECTION ( 'NONE',  ( 0.000000000000000000, 0.000000000000000000, -1.000000000000000000 ) ) ;
#7342 = VECTOR ( 'NONE', #7757, 1000.000000000000000 ) ;
#7343 = PLANE ( 'NONE',  #7355 ) ;
#7344 = VERTEX_POINT ( 'NONE', #8343 ) ;
#7345 = AXIS2_PLACEMENT_3D ( 'NONE', #15302, #4501, #3404 ) ;
#7346 = CIRCLE ( 'NONE', #10565, 3.524999999999998579 ) ;
#7347 = EDGE_LOOP ( 'NONE', ( #9765, #5857, #13236, #5992 ) ) ;
#7348 = DIRECTION ( 'NONE',  ( 0.000000000000000000, 0.000000000000000000, -1.000000000000000000 ) ) ;
#7349 = DIRECTION ( 'NONE',  ( 0.000000000000000000, 0.000000000000000000, -1.000000000000000000 ) ) ;
#7350 = DIRECTION ( 'NONE',  ( 0.000000000000000000, 0.000000000000000000, -1.000000000000000000 ) ) ;
#7351 = DIRECTION ( 'NONE',  ( 0.000000000000000000, 0.000000000000000000, 1.000000000000000000 ) ) ;
#7352 = CARTESIAN_POINT ( 'NONE',  ( 115.7000000000000597, 62.13993994372673768, 15.00000000000035172 ) ) ;
#7353 = CARTESIAN_POINT ( 'NONE',  ( 17.41029453487719181, 40.04259805664093363, 0.000000000000000000 ) ) ;
#7354 = CARTESIAN_POINT ( 'NONE',  ( -193.7244371550166022, 142.0541455854551600, 3.478855109513427468 ) ) ;
#7355 = AXIS2_PLACEMENT_3D ( 'NONE', #12059, #5112, #1236 ) ;
#7356 = ORIENTED_EDGE ( 'NONE', *, *, #12725, .F. ) ;
#7357 = VECTOR ( 'NONE', #9065, 1000.000000000000000 ) ;
#7358 = EDGE_CURVE ( 'NONE', #13697, #14280, #8801, .T. ) ;
#7359 = ORIENTED_EDGE ( 'NONE', *, *, #3199, .T. ) ;
#7360 = FACE_OUTER_BOUND ( 'NONE', #8611, .T. ) ;
#7361 = ORIENTED_EDGE ( 'NONE', *, *, #15375, .T. ) ;
#7362 = CARTESIAN_POINT ( 'NONE',  ( -225.6149816284549559, 143.0145576275852193, 4.031212713769876999 ) ) ;
#7363 = ORIENTED_EDGE ( 'NONE', *, *, #889, .F. ) ;
#7364 = DIRECTION ( 'NONE',  ( 1.000000000000000000, 0.000000000000000000, 0.000000000000000000 ) ) ;
#7365 = CARTESIAN_POINT ( 'NONE',  ( 211.8948836958790594, 42.45667055239124466, -1.443217624331801563 ) ) ;
#7366 = AXIS2_PLACEMENT_3D ( 'NONE', #614, #10265, #6491 ) ;
#7367 = ORIENTED_EDGE ( 'NONE', *, *, #10292, .T. ) ;
#7368 = LINE ( 'NONE', #1183, #10798 ) ;
#7369 = CARTESIAN_POINT ( 'NONE',  ( 177.5000000000000853, 17.53993994372674692, -17.50000000000002487 ) ) ;
#7370 =( GEOMETRIC_REPRESENTATION_CONTEXT ( 3 ) GLOBAL_UNCERTAINTY_ASSIGNED_CONTEXT ( ( #15096 ) ) GLOBAL_UNIT_ASSIGNED_CONTEXT ( ( #10146, #3971, #5694 ) ) REPRESENTATION_CONTEXT ( 'NONE', 'WORKASPACE' ) );
#7371 = ADVANCED_FACE ( 'NONE', ( #13364 ), #7311, .F. ) ;
#7372 = FACE_OUTER_BOUND ( 'NONE', #5056, .T. ) ;
#7373 = VERTEX_POINT ( 'NONE', #1286 ) ;
#7374 = AXIS2_PLACEMENT_3D ( 'NONE', #1062, #4773, #15335 ) ;
#7375 = ORIENTED_EDGE ( 'NONE', *, *, #5440, .F. ) ;
#7376 = CARTESIAN_POINT ( 'NONE',  ( 190.5000000000000568, 19.53993994372674692, -17.50000000000002487 ) ) ;
#7377 = AXIS2_PLACEMENT_3D ( 'NONE', #6873, #14418, #3616 ) ;
#7378 = EDGE_LOOP ( 'NONE', ( #14938, #1616, #11470, #7682 ) ) ;
#7379 = CARTESIAN_POINT ( 'NONE',  ( 177.5000000000000853, -178.6666270497714777, 53.18093594598651919 ) ) ;
#7380 = CARTESIAN_POINT ( 'NONE',  ( -85.99999999999994316, 62.13993994372673768, 15.00000000000174794 ) ) ;
#7381 = CARTESIAN_POINT ( 'NONE',  ( -152.3848650261365663, 107.5241111436813242, -4.636096941365081214 ) ) ;
#7382 = ORIENTED_EDGE ( 'NONE', *, *, #12403, .T. ) ;
#7383 = ORIENTED_EDGE ( 'NONE', *, *, #2749, .T. ) ;
#7384 = CARTESIAN_POINT ( 'NONE',  ( -215.0356418556126812, 153.5741063705486908, -0.4547266291960771478 ) ) ;
#7385 = EDGE_CURVE ( 'NONE', #2732, #11374, #4768, .T. ) ;
#7386 = CARTESIAN_POINT ( 'NONE',  ( 193.0950460371283839, 35.57958264137020876, -2.685405722344195389 ) ) ;
#7387 = ORIENTED_EDGE ( 'NONE', *, *, #7802, .F. ) ;
#7388 = PRESENTATION_LAYER_ASSIGNMENT (  '', '', ( #5355 ) ) ;
#7389 = CARTESIAN_POINT ( 'NONE',  ( 184.0000000000000568, -179.3058001507315566, 76.45141194869098911 ) ) ;
#7390 = DIRECTION ( 'NONE',  ( 0.8731965799097684000, -0.4873681696970816324, -0.000000000000000000 ) ) ;
#7391 = AXIS2_PLACEMENT_3D ( 'NONE', #5198, #5352, #1473 ) ;
#7392 = LINE ( 'NONE', #12183, #2243 ) ;
#7393 = ORIENTED_EDGE ( 'NONE', *, *, #14218, .F. ) ;
#7394 = EDGE_CURVE ( 'NONE', #8350, #12412, #3019, .T. ) ;
#7395 = DIRECTION ( 'NONE',  ( 0.8731965799097690661, -0.4873681696970805222, 0.000000000000000000 ) ) ;
#7396 = CARTESIAN_POINT ( 'NONE',  ( 188.3076603040395582, 42.49356297222218615, -1.493920802967548367 ) ) ;
#7397 = ORIENTED_EDGE ( 'NONE', *, *, #9435, .T. ) ;
#7398 = CARTESIAN_POINT ( 'NONE',  ( -63.50000000000002842, -178.6666270497714777, 53.18093594598651919 ) ) ;
#7399 = DIRECTION ( 'NONE',  ( -3.965082230804130220E-16, 0.000000000000000000, 1.000000000000000000 ) ) ;
#7400 = CARTESIAN_POINT ( 'NONE',  ( -188.3338018137096128, 131.5603057966125675, -5.230826428279604201 ) ) ;
#7401 = CARTESIAN_POINT ( 'NONE',  ( 64.00000000000005684, 56.53993994372675047, 16.70000000000069562 ) ) ;
#7402 = EDGE_LOOP ( 'NONE', ( #12447, #7068, #15328, #12018 ) ) ;
#7403 = CARTESIAN_POINT ( 'NONE',  ( -182.2596580518439850, 130.2653702959948987, 9.578254705571840333 ) ) ;
#7404 = CIRCLE ( 'NONE', #5620, 1.499999999999994449 ) ;
#7405 = DIRECTION ( 'NONE',  ( -1.000000000000000000, -0.000000000000000000, -0.000000000000000000 ) ) ;
#7406 = VERTEX_POINT ( 'NONE', #9591 ) ;
#7407 = EDGE_LOOP ( 'NONE', ( #6196, #2633, #12833, #8617 ) ) ;
#7408 = DIRECTION ( 'NONE',  ( 1.000000000000000000, 0.000000000000000000, 0.000000000000000000 ) ) ;
#7409 = AXIS2_PLACEMENT_3D ( 'NONE', #10194, #6725, #11375 ) ;
#7410 = CARTESIAN_POINT ( 'NONE',  ( 0.3194001229790410235, 3.115132258388565667, 8.000000000000007105 ) ) ;
#7411 = CARTESIAN_POINT ( 'NONE',  ( 172.5293059057019889, 61.25683321636181233, 0.000000000000000000 ) ) ;
#7412 = CYLINDRICAL_SURFACE ( 'NONE', #754, 1.700000000000007061 ) ;
#7413 = AXIS2_PLACEMENT_3D ( 'NONE', #1405, #5360, #6238 ) ;
#7414 = EDGE_CURVE ( 'NONE', #6288, #14252, #982, .T. ) ;
#7415 = CARTESIAN_POINT ( 'NONE',  ( 185.1062858801516882, 55.86394065090267702, 18.00000000000000355 ) ) ;
#7417 = EDGE_CURVE ( 'NONE', #2673, #2210, #9574, .T. ) ;
#7416 = EDGE_CURVE ( 'NONE', #163, #2412, #14389, .T. ) ;
#7418 = CARTESIAN_POINT ( 'NONE',  ( 114.0000000000000568, 64.53993994372673626, 15.00000000000035172 ) ) ;
#7419 = LINE ( 'NONE', #1235, #3985 ) ;
#7420 = CARTESIAN_POINT ( 'NONE',  ( 51.07686401294030532, 368.7106150007013525, 5.000000000000000000 ) ) ;
#7421 = ORIENTED_EDGE ( 'NONE', *, *, #10976, .T. ) ;
#7422 = ORIENTED_EDGE ( 'NONE', *, *, #4767, .T. ) ;
#7423 = DIRECTION ( 'NONE',  ( 1.000000000000000000, 0.000000000000000000, 0.000000000000000000 ) ) ;
#7424 = DIRECTION ( 'NONE',  ( -1.000000000000000000, -0.000000000000000000, -0.000000000000000000 ) ) ;
#7425 = SURFACE_STYLE_FILL_AREA ( #13239 ) ;
#7426 = DIRECTION ( 'NONE',  ( 0.000000000000000000, 0.5000000000000013323, 0.8660254037844380415 ) ) ;
#7427 = CARTESIAN_POINT ( 'NONE',  ( 178.0000000000000853, 15.10952649420676863, 9.557440204760682789 ) ) ;
#7428 = FACE_OUTER_BOUND ( 'NONE', #4577, .T. ) ;
#7429 = CARTESIAN_POINT ( 'NONE',  ( 2.000000000000000000, -1.587713240271472648, -2.750000000000000888 ) ) ;
#7430 = AXIS2_PLACEMENT_3D ( 'NONE', #8666, #14558, #12200 ) ;
#7431 = ORIENTED_EDGE ( 'NONE', *, *, #3981, .F. ) ;
#7432 = TOROIDAL_SURFACE ( 'NONE', #4903, 6.999999999999991118, 2.000000000000000000 ) ;
#7433 = CARTESIAN_POINT ( 'NONE',  ( 198.7876695280922661, 49.53587328158837977, -8.249370650301745655 ) ) ;
#7434 = FACE_OUTER_BOUND ( 'NONE', #5010, .T. ) ;
#7435 = ORIENTED_EDGE ( 'NONE', *, *, #9636, .F. ) ;
#7436 = CARTESIAN_POINT ( 'NONE',  ( -222.2306213242449360, 149.0781703675127403, 7.930418395707709678 ) ) ;
#7437 = EDGE_LOOP ( 'NONE', ( #13822, #9100, #4483, #8609 ) ) ;
#7438 = CARTESIAN_POINT ( 'NONE',  ( -168.9408230362998893, 125.5486682295035905, -3.359583683245268126 ) ) ;
#7439 = CARTESIAN_POINT ( 'NONE',  ( -130.0135953313997561, 106.9229804370480537, 5.000000000000000000 ) ) ;
#7440 = ORIENTED_EDGE ( 'NONE', *, *, #3383, .T. ) ;
#7441 = DIRECTION ( 'NONE',  ( 0.000000000000000000, 0.000000000000000000, 1.000000000000000000 ) ) ;
#7442 = LINE ( 'NONE', #14291, #14108 ) ;
#7443 = EDGE_CURVE ( 'NONE', #5773, #11153, #2774, .T. ) ;
#7444 = AXIS2_PLACEMENT_3D ( 'NONE', #11502, #11574, #4299 ) ;
#7445 = DIRECTION ( 'NONE',  ( 0.000000000000000000, 0.000000000000000000, -1.000000000000000000 ) ) ;
#7446 = ORIENTED_EDGE ( 'NONE', *, *, #13549, .T. ) ;
#7447 = SHAPE_DEFINITION_REPRESENTATION ( #12800, #13652 ) ;
#7448 = EDGE_LOOP ( 'NONE', ( #5144, #5562 ) ) ;
#7449 = PRESENTATION_STYLE_ASSIGNMENT (( #14685 ) ) ;
#7450 = ORIENTED_EDGE ( 'NONE', *, *, #1397, .F. ) ;
#7451 = CARTESIAN_POINT ( 'NONE',  ( 14.00000000000004086, 62.13993994372673768, 15.00000000000104983 ) ) ;
#7452 = AXIS2_PLACEMENT_3D ( 'NONE', #8969, #12889, #1994 ) ;
#7453 = CARTESIAN_POINT ( 'NONE',  ( 203.4093511297050725, 50.30250970312702208, -0.9107274384406883749 ) ) ;
#7454 = VERTEX_POINT ( 'NONE', #15 ) ;
#7455 = VERTEX_POINT ( 'NONE', #2327 ) ;
#7456 = CARTESIAN_POINT ( 'NONE',  ( -180.9555975561403613, 132.5588568579215973, -2.963320117457099112 ) ) ;
#7457 = CARTESIAN_POINT ( 'NONE',  ( 205.4319281802536068, 33.87189768065903905, -1.932853472788024440 ) ) ;
#7458 = ORIENTED_EDGE ( 'NONE', *, *, #7991, .F. ) ;
#7459 = CARTESIAN_POINT ( 'NONE',  ( -156.3654661690580667, 109.2025351267266586, -4.449251264896256330 ) ) ;
#7460 = CARTESIAN_POINT ( 'NONE',  ( -222.0995690897442785, 149.3129710173510318, 2.431557144026069928 ) ) ;
#7461 = CARTESIAN_POINT ( 'NONE',  ( 14.00000000000004086, 64.53993994372673626, 15.00000000000104983 ) ) ;
#7462 = AXIS2_PLACEMENT_3D ( 'NONE', #12095, #13503, #3728 ) ;
#7463 = AXIS2_PLACEMENT_3D ( 'NONE', #11242, #12105, #13441 ) ;
#7464 = ADVANCED_FACE ( 'NONE', ( #2401 ), #4856, .F. ) ;
#7465 = FACE_BOUND ( 'NONE', #6355, .T. ) ;
#7466 = CARTESIAN_POINT ( 'NONE',  ( 207.1782284445936284, 46.06712597851176838, -2.617760425820522041 ) ) ;
#7467 = VERTEX_POINT ( 'NONE', #7236 ) ;
#7468 = DIRECTION ( 'NONE',  ( -0.000000000000000000, -0.000000000000000000, 1.000000000000000000 ) ) ;
#7469 = CARTESIAN_POINT ( 'NONE',  ( -218.9522465171050953, 150.9009417352626770, -4.531563180531605006 ) ) ;
#7470 = CARTESIAN_POINT ( 'NONE',  ( -174.6098962832414827, 120.3911030166530054, -4.778074536717329401 ) ) ;
#7471 = FACE_OUTER_BOUND ( 'NONE', #14129, .T. ) ;
#7472 = EDGE_LOOP ( 'NONE', ( #11933, #14057, #4077, #6758, #12596, #8404 ) ) ;
#7473 = CARTESIAN_POINT ( 'NONE',  ( -183.7478807014743722, 127.6480629723144347, 10.16010209732750624 ) ) ;
#7474 = CARTESIAN_POINT ( 'NONE',  ( 207.1164837741930569, 35.57719129110033407, -1.806778302941847159 ) ) ;
#7475 = CIRCLE ( 'NONE', #15011, 1.699999999999993072 ) ;
#7476 = ORIENTED_EDGE ( 'NONE', *, *, #8722, .F. ) ;
#7477 = EDGE_LOOP ( 'NONE', ( #12176, #4081 ) ) ;
#7478 = ADVANCED_FACE ( 'NONE', ( #1437 ), #8497, .T. ) ;
#7479 = CARTESIAN_POINT ( 'NONE',  ( 17.41029453487719181, 40.04259805664093363, 9.975000000000001421 ) ) ;
#7480 = CARTESIAN_POINT ( 'NONE',  ( -76.00000000000001421, 15.03993994372673804, 24.94742576086838781 ) ) ;
#7481 = CARTESIAN_POINT ( 'NONE',  ( -225.2945142095777840, 143.5887253133888635, -1.007486474111332075 ) ) ;
#7482 = CARTESIAN_POINT ( 'NONE',  ( -85.99999999999994316, 62.13993994372673768, 18.50000000000175149 ) ) ;
#7483 = CARTESIAN_POINT ( 'NONE',  ( 0.000000000000000000, 2.381569860407204420, 1.375000000000001110 ) ) ;
#7484 = VECTOR ( 'NONE', #5648, 1000.000000000000000 ) ;
#7485 = CARTESIAN_POINT ( 'NONE',  ( -192.3703904092303105, 140.8200239622036918, 5.434754235172604808 ) ) ;
#7486 = DIRECTION ( 'NONE',  ( -3.965082230804130220E-16, 0.000000000000000000, 1.000000000000000000 ) ) ;
#7487 = LINE ( 'NONE', #12212, #5601 ) ;
#7488 = ORIENTED_EDGE ( 'NONE', *, *, #14518, .F. ) ;
#7489 = ADVANCED_FACE ( 'NONE', ( #8568 ), #15491, .F. ) ;
#7490 = CARTESIAN_POINT ( 'NONE',  ( 166.9217645774054120, 62.57671370024034729, -0.9107274384406883749 ) ) ;
#7491 = ORIENTED_EDGE ( 'NONE', *, *, #9969, .T. ) ;
#7492 = LINE ( 'NONE', #14962, #13425 ) ;
#7493 = DIRECTION ( 'NONE',  ( 0.000000000000000000, -1.000000000000000000, -6.938893903907227145E-17 ) ) ;
#7494 = DIRECTION ( 'NONE',  ( 3.965082230804130220E-16, -0.000000000000000000, -1.000000000000000000 ) ) ;
#7495 = CARTESIAN_POINT ( 'NONE',  ( 20.91029453487719181, 40.04259805664093363, 9.975000000000001421 ) ) ;
#7496 = APPLICATION_CONTEXT ( 'automotive_design' ) ;
#7497 = CARTESIAN_POINT ( 'NONE',  ( 5.799999999999999822, 4.618802153516981868, -7.999999999999979572 ) ) ;
#7498 = DIRECTION ( 'NONE',  ( -0.000000000000000000, -0.000000000000000000, -1.000000000000000000 ) ) ;
#7499 = EDGE_CURVE ( 'NONE', #13870, #11107, #213, .T. ) ;
#7500 = EDGE_CURVE ( 'NONE', #10298, #2939, #9076, .T. ) ;
#7501 = CYLINDRICAL_SURFACE ( 'NONE', #14854, 1.500000000000001332 ) ;
#7502 = CARTESIAN_POINT ( 'NONE',  ( -186.0759242617834559, 135.7072545306847076, 7.919662025281895446 ) ) ;
#7503 = EDGE_CURVE ( 'NONE', #13002, #8697, #15102, .T. ) ;
#7504 = ORIENTED_EDGE ( 'NONE', *, *, #7414, .F. ) ;
#7505 = DIRECTION ( 'NONE',  ( 1.000000000000000000, 0.000000000000000000, 0.000000000000000000 ) ) ;
#7506 = CARTESIAN_POINT ( 'NONE',  ( 178.0000000000000853, -179.8058001507315566, -30.31842631998718574 ) ) ;
#7507 = CARTESIAN_POINT ( 'NONE',  ( -219.4360840196855804, 154.0850226169901305, 3.058976617611859794 ) ) ;
#7508 = EDGE_LOOP ( 'NONE', ( #13661, #13253 ) ) ;
#7509 = CARTESIAN_POINT ( 'NONE',  ( -218.5426395586106025, 155.6857686161635286, 4.229107391422298967 ) ) ;
#7510 = ORIENTED_EDGE ( 'NONE', *, *, #12304, .T. ) ;
#7511 = CARTESIAN_POINT ( 'NONE',  ( 51.07686401294030532, 368.7106150007013525, 5.000000000000000000 ) ) ;
#7512 = DIRECTION ( 'NONE',  ( 3.965082230804130220E-16, 1.090924371466202084E-47, 1.000000000000000000 ) ) ;
#7513 = EDGE_CURVE ( 'NONE', #12769, #11977, #5958, .T. ) ;
#7514 = ORIENTED_EDGE ( 'NONE', *, *, #14792, .T. ) ;
#7515 = EDGE_CURVE ( 'NONE', #828, #4926, #8070, .T. ) ;
#7516 = DIRECTION ( 'NONE',  ( 8.659560562354932858E-17, 0.7071067811865474617, -0.7071067811865474617 ) ) ;
#7517 = CARTESIAN_POINT ( 'NONE',  ( 5.196152422706635576, -9.000000000000003553, 5.000000000000000000 ) ) ;
#7518 = AXIS2_PLACEMENT_3D ( 'NONE', #2357, #3695, #11994 ) ;
#7519 = DIRECTION ( 'NONE',  ( -1.000000000000000000, -0.000000000000000000, -0.000000000000000000 ) ) ;
#7520 = ORIENTED_EDGE ( 'NONE', *, *, #2314, .F. ) ;
#7521 = AXIS2_PLACEMENT_3D ( 'NONE', #13579, #11383, #461 ) ;
#7522 = DIRECTION ( 'NONE',  ( 1.156482317317871725E-16, 1.156482317317871725E-16, -1.000000000000000000 ) ) ;
#7523 = ORIENTED_EDGE ( 'NONE', *, *, #14249, .F. ) ;
#7524 = DIRECTION ( 'NONE',  ( 0.000000000000000000, 1.156482317317871478E-16, -1.000000000000000000 ) ) ;
#7525 = CARTESIAN_POINT ( 'NONE',  ( 51.07686401294030532, 368.7106150007013525, 5.000000000000000000 ) ) ;
#7526 = ORIENTED_EDGE ( 'NONE', *, *, #10428, .F. ) ;
#7527 = CARTESIAN_POINT ( 'NONE',  ( -76.00000000000001421, -178.8058001507315566, 52.19066787724494816 ) ) ;
#7528 = EDGE_CURVE ( 'NONE', #8873, #9626, #10591, .T. ) ;
#7529 = AXIS2_PLACEMENT_3D ( 'NONE', #6778, #4313, #14022 ) ;
#7530 = CARTESIAN_POINT ( 'NONE',  ( -151.9357463660236078, 108.1326792441745255, -4.859112388478815880 ) ) ;
#7531 = EDGE_LOOP ( 'NONE', ( #13358, #8710, #15582, #10417 ) ) ;
#7532 = VERTEX_POINT ( 'NONE', #12564 ) ;
#7533 = CARTESIAN_POINT ( 'NONE',  ( -63.50000000000002842, -179.3058001507315566, -17.19066787724516843 ) ) ;
#7534 = CARTESIAN_POINT ( 'NONE',  ( 194.7957337413261030, 33.86335648926068842, -5.558215102112974648 ) ) ;
#7535 = AXIS2_PLACEMENT_3D ( 'NONE', #501, #587, #12515 ) ;
#7536 = EDGE_LOOP ( 'NONE', ( #13813, #7967 ) ) ;
#7537 = DIRECTION ( 'NONE',  ( 0.000000000000000000, 0.1391731009600660485, -0.9902680687415702510 ) ) ;
#7538 = CARTESIAN_POINT ( 'NONE',  ( 178.0000000000000853, -179.3058001507315566, 65.31842631998698323 ) ) ;
#7539 = DIRECTION ( 'NONE',  ( 1.000000000000000000, 0.000000000000000000, 0.000000000000000000 ) ) ;
#7540 = AXIS2_PLACEMENT_3D ( 'NONE', #12714, #7930, #13020 ) ;
#7541 = AXIS2_PLACEMENT_3D ( 'NONE', #8116, #12903, #14237 ) ;
#7542 = VECTOR ( 'NONE', #11892, 1000.000000000000000 ) ;
#7543 = SURFACE_SIDE_STYLE ('',( #7314 ) ) ;
#7544 = EDGE_CURVE ( 'NONE', #1809, #5430, #4795, .T. ) ;
#7545 = CARTESIAN_POINT ( 'NONE',  ( 209.6356879938037139, 47.96904352876332922, -5.622739983145865317 ) ) ;
#7546 = ORIENTED_EDGE ( 'NONE', *, *, #72, .T. ) ;
#7547 = FACE_BOUND ( 'NONE', #1340, .T. ) ;
#7548 = CARTESIAN_POINT ( 'NONE',  ( -83.57455057502457407, 65.19100426474074084, 7.600000000000002309 ) ) ;
#7549 = CARTESIAN_POINT ( 'NONE',  ( -217.2107590478593977, 140.9839873040922100, -2.964974570226843742 ) ) ;
#7550 = CYLINDRICAL_SURFACE ( 'NONE', #1225, 1.499999999999994449 ) ;
#7551 = ORIENTED_EDGE ( 'NONE', *, *, #7569, .T. ) ;
#7552 = CARTESIAN_POINT ( 'NONE',  ( -209.4369489341841586, 132.9646294043573675, 3.478895870929508582 ) ) ;
#7553 = CARTESIAN_POINT ( 'NONE',  ( 201.3910773252651438, 49.55986643532389735, -5.240523689774838623 ) ) ;
#7554 = EDGE_LOOP ( 'NONE', ( #7893, #4228, #5298, #5591 ) ) ;
#7555 = ORIENTED_EDGE ( 'NONE', *, *, #8743, .F. ) ;
#7556 = CIRCLE ( 'NONE', #13069, 1.699999999999994849 ) ;
#7557 = TOROIDAL_SURFACE ( 'NONE', #12073, 1.000000000000000000, 0.5000000000000000000 ) ;
#7558 = AXIS2_PLACEMENT_3D ( 'NONE', #5873, #8257, #6989 ) ;
#7559 = CARTESIAN_POINT ( 'NONE',  ( 0.4964154566687650205, -4.996589667937459289, -7.345652830558652369 ) ) ;
#7560 = DIRECTION ( 'NONE',  ( 1.000000000000000000, 0.000000000000000000, 0.000000000000000000 ) ) ;
#7561 = DIRECTION ( 'NONE',  ( 0.4873681696970831312, 0.8731965799097676229, 0.000000000000000000 ) ) ;
#7562 = AXIS2_PLACEMENT_3D ( 'NONE', #6679, #11484, #8015 ) ;
#7563 = FACE_OUTER_BOUND ( 'NONE', #14127, .T. ) ;
#7564 = CARTESIAN_POINT ( 'NONE',  ( 194.0000000000000568, 59.53993994372674337, 10.00000000000000178 ) ) ;
#7565 = CARTESIAN_POINT ( 'NONE',  ( -173.3366878899875019, 128.3846004176512849, 7.899914667150486736 ) ) ;
#7566 = CARTESIAN_POINT ( 'NONE',  ( 178.0000000000000853, 15.03993994372673981, -3.075184203610571654 ) ) ;
#7567 = CARTESIAN_POINT ( 'NONE',  ( -70.00000000000000000, 17.53993994372673981, -12.49999999999999467 ) ) ;
#7568 = EDGE_LOOP ( 'NONE', ( #32, #10944, #14925, #5467 ) ) ;
#7569 = EDGE_CURVE ( 'NONE', #9150, #4749, #5237, .T. ) ;
#7570 = PLANE ( 'NONE',  #14379 ) ;
#7571 = ORIENTED_EDGE ( 'NONE', *, *, #9662, .T. ) ;
#7572 = ORIENTED_EDGE ( 'NONE', *, *, #12429, .T. ) ;
#7573 = AXIS2_PLACEMENT_3D ( 'NONE', #9292, #15192, #1068 ) ;
#7574 = CARTESIAN_POINT ( 'NONE',  ( -76.00000000000001421, 15.53993994372673981, -2.500000000000071054 ) ) ;
#7575 = LINE ( 'NONE', #8753, #950 ) ;
#7576 = CIRCLE ( 'NONE', #13089, 1.000000000000000888 ) ;
#7577 = DIRECTION ( 'NONE',  ( 0.000000000000000000, -1.000000000000000000, 0.000000000000000000 ) ) ;
#7578 = CIRCLE ( 'NONE', #8580, 0.5000000000000004441 ) ;
#7579 = CARTESIAN_POINT ( 'NONE',  ( 224.0000000000000853, 19.53993994372674337, 24.99999999999999645 ) ) ;
#7580 = DIRECTION ( 'NONE',  ( -3.965082230804130220E-16, 4.956352788505162775E-17, -1.000000000000000000 ) ) ;
#7581 = DIRECTION ( 'NONE',  ( -0.000000000000000000, -0.000000000000000000, 1.000000000000000000 ) ) ;
#7582 = CARTESIAN_POINT ( 'NONE',  ( -180.1381104688653920, 133.9928400706745037, 5.434754235172599479 ) ) ;
#7584 = ORIENTED_EDGE ( 'NONE', *, *, #549, .T. ) ;
#7583 = EDGE_CURVE ( 'NONE', #61, #259, #6358, .T. ) ;
#7585 = VECTOR ( 'NONE', #12164, 1000.000000000000000 ) ;
#7586 = VECTOR ( 'NONE', #6718, 1000.000000000000000 ) ;
#7587 = EDGE_CURVE ( 'NONE', #12236, #12329, #11340, .T. ) ;
#7588 = AXIS2_PLACEMENT_3D ( 'NONE', #11984, #1154, #7257 ) ;
#7589 = CARTESIAN_POINT ( 'NONE',  ( 198.9111841706756536, 32.15857605477618364, -5.308824953579920347 ) ) ;
#7590 = CARTESIAN_POINT ( 'NONE',  ( -219.4552112669440191, 154.0507531510554884, 3.411777084580434938 ) ) ;
#7591 = ORIENTED_EDGE ( 'NONE', *, *, #7513, .T. ) ;
#7592 = CARTESIAN_POINT ( 'NONE',  ( -218.6814998127593412, 155.4369786734033880, 5.141710482893284251 ) ) ;
#7593 = ORIENTED_EDGE ( 'NONE', *, *, #10181, .F. ) ;
#7594 = DIRECTION ( 'NONE',  ( -0.000000000000000000, -0.000000000000000000, 1.000000000000000000 ) ) ;
#7595 = CARTESIAN_POINT ( 'NONE',  ( 203.8258924691278082, 51.74121150033466421, -0.9185252821640312870 ) ) ;
#7596 = ORIENTED_EDGE ( 'NONE', *, *, #5172, .F. ) ;
#7597 = CARTESIAN_POINT ( 'NONE',  ( -150.4352220630557895, 107.0097505318674393, 9.657855017614867421 ) ) ;
#7598 = DIRECTION ( 'NONE',  ( -0.000000000000000000, -0.000000000000000000, 1.000000000000000000 ) ) ;
#7599 = AXIS2_PLACEMENT_3D ( 'NONE', #4026, #14983, #7679 ) ;
#7600 = AXIS2_PLACEMENT_3D ( 'NONE', #13541, #2747, #8678 ) ;
#7601 = CARTESIAN_POINT ( 'NONE',  ( -70.00000000000000000, 15.53993994372673626, 47.49999999999997868 ) ) ;
#7602 = EDGE_LOOP ( 'NONE', ( #13510, #8501, #2559, #10727 ) ) ;
#7603 = DIRECTION ( 'NONE',  ( 0.000000000000000000, -1.000000000000000000, 0.000000000000000000 ) ) ;
#7604 = ORIENTED_EDGE ( 'NONE', *, *, #8947, .F. ) ;
#7605 = ADVANCED_FACE ( 'NONE', ( #3900 ), #14855, .F. ) ;
#7606 = ADVANCED_FACE ( 'NONE', ( #242 ), #1503, .T. ) ;
#7607 = CARTESIAN_POINT ( 'NONE',  ( 190.5000000000000853, 16.03993994372673626, 38.07518420361041933 ) ) ;
#7608 = EDGE_CURVE ( 'NONE', #2275, #3552, #2716, .T. ) ;
#7609 = CARTESIAN_POINT ( 'NONE',  ( 73.79035645333922844, 38.79159067395544014, 10.00000000000000178 ) ) ;
#7610 = ORIENTED_EDGE ( 'NONE', *, *, #203, .T. ) ;
#7611 = FACE_OUTER_BOUND ( 'NONE', #12367, .T. ) ;
#7612 = CIRCLE ( 'NONE', #13894, 3.500000000000001332 ) ;
#7613 = FACE_OUTER_BOUND ( 'NONE', #2791, .T. ) ;
#7614 = ORIENTED_EDGE ( 'NONE', *, *, #10764, .F. ) ;
#7615 = ORIENTED_EDGE ( 'NONE', *, *, #2102, .F. ) ;
#7616 = AXIS2_PLACEMENT_3D ( 'NONE', #7318, #11096, #4937 ) ;
#7617 = CARTESIAN_POINT ( 'NONE',  ( 169.1145417280692698, 64.59938046134368506, -0.9107274384406877088 ) ) ;
#7618 = DIRECTION ( 'NONE',  ( 1.000000000000000000, 0.000000000000000000, -0.000000000000000000 ) ) ;
#7619 = VERTEX_POINT ( 'NONE', #2879 ) ;
#7620 = DIRECTION ( 'NONE',  ( -0.09810338464376283651, -0.9951762285753403825, 0.000000000000000000 ) ) ;
#7621 = CARTESIAN_POINT ( 'NONE',  ( -155.7734221399892363, 109.6948923088348806, -4.718200141660416236 ) ) ;
#7622 = DIRECTION ( 'NONE',  ( -0.8731965799097686221, 0.4873681696970811883, 0.000000000000000000 ) ) ;
#7623 = DIRECTION ( 'NONE',  ( 0.000000000000000000, -0.9902680687415702510, 0.1391731009600660485 ) ) ;
#7624 = VECTOR ( 'NONE', #15601, 1000.000000000000114 ) ;
#7625 = ADVANCED_FACE ( 'NONE', ( #12649 ), #3968, .F. ) ;
#7626 = VECTOR ( 'NONE', #4734, 1000.000000000000000 ) ;
#7627 = ORIENTED_EDGE ( 'NONE', *, *, #7017, .T. ) ;
#7628 = CARTESIAN_POINT ( 'NONE',  ( 172.5293059057019889, 61.25683321636181233, 10.00000000000000178 ) ) ;
#7629 = CARTESIAN_POINT ( 'NONE',  ( -217.1265240672488233, 154.1501268790366339, -1.115935190456407433 ) ) ;
#7630 = CARTESIAN_POINT ( 'NONE',  ( -181.9037801448002938, 118.7381910193847716, -0.5218507872395746761 ) ) ;
#7631 = DIRECTION ( 'NONE',  ( 0.000000000000000000, 0.000000000000000000, 1.000000000000000000 ) ) ;
#7632 = ORIENTED_EDGE ( 'NONE', *, *, #2223, .T. ) ;
#7633 = CARTESIAN_POINT ( 'NONE',  ( -221.7331157600676192, 141.5908957077777188, 3.478895870929496148 ) ) ;
#7635 = CARTESIAN_POINT ( 'NONE',  ( 201.1780093772972009, 32.12620995903681376, -3.617034841014101776 ) ) ;
#7634 = TOROIDAL_SURFACE ( 'NONE', #7374, 1.000000000000000000, 0.5000000000000000000 ) ;
#7636 = ORIENTED_EDGE ( 'NONE', *, *, #8600, .T. ) ;
#7637 = CARTESIAN_POINT ( 'NONE',  ( -76.50000000000001421, -179.8058001507315566, -29.88378295107906624 ) ) ;
#7638 = CARTESIAN_POINT ( 'NONE',  ( -35.99999999999995026, 62.13993994372673768, 15.00000000000139977 ) ) ;
#7639 = EDGE_CURVE ( 'NONE', #2454, #11537, #6316, .T. ) ;
#7640 = EDGE_CURVE ( 'NONE', #13140, #234, #9090, .T. ) ;
#7641 = DIRECTION ( 'NONE',  ( 1.000000000000000000, 2.751328491981765035E-32, -3.965082230804130220E-16 ) ) ;
#7642 = EDGE_CURVE ( 'NONE', #2814, #15158, #15608, .T. ) ;
#7643 = CARTESIAN_POINT ( 'NONE',  ( 5.799999999999999822, 7.999999999999979572, 0.000000000000000000 ) ) ;
#7644 = AXIS2_PLACEMENT_3D ( 'NONE', #6018, #14525, #11867 ) ;
#7645 = EDGE_LOOP ( 'NONE', ( #11145, #6578, #3628, #13347 ) ) ;
#7646 = DIRECTION ( 'NONE',  ( -0.000000000000000000, -0.000000000000000000, 1.000000000000000000 ) ) ;
#7647 = CARTESIAN_POINT ( 'NONE',  ( -180.1381104688653920, 133.9928400706745037, 5.434754235172599479 ) ) ;
#7648 = DIRECTION ( 'NONE',  ( 0.000000000000000000, -1.000000000000000000, 0.000000000000000000 ) ) ;
#7649 = CARTESIAN_POINT ( 'NONE',  ( -157.5299867052495699, 110.6848347650430782, -4.720820933574413125 ) ) ;
#7650 = VERTEX_POINT ( 'NONE', #11243 ) ;
#7651 = DIRECTION ( 'NONE',  ( 0.000000000000000000, 0.000000000000000000, 1.000000000000000000 ) ) ;
#7652 = ORIENTED_EDGE ( 'NONE', *, *, #2238, .T. ) ;
#7653 = ORIENTED_EDGE ( 'NONE', *, *, #9139, .T. ) ;
#7654 = DIRECTION ( 'NONE',  ( 3.965082230804130220E-16, 0.000000000000000000, 1.000000000000000000 ) ) ;
#7655 = CARTESIAN_POINT ( 'NONE',  ( -10.39230484541326582, 4.570335331080236228E-16, 5.000000000000000000 ) ) ;
#7656 = CARTESIAN_POINT ( 'NONE',  ( 164.0000000000000568, 56.53993994372675047, 15.00000000000000355 ) ) ;
#7657 = DIRECTION ( 'NONE',  ( -0.000000000000000000, 0.8660254037844391517, 0.4999999999999991673 ) ) ;
#7658 = DIRECTION ( 'NONE',  ( -1.000000000000000000, 0.000000000000000000, 0.000000000000000000 ) ) ;
#7659 = CARTESIAN_POINT ( 'NONE',  ( -218.7271737403003442, 151.3100222557285122, -4.321910846754870583 ) ) ;
#7660 = CARTESIAN_POINT ( 'NONE',  ( -199.6024142766798946, 142.8729305612646385, 7.919662025281897222 ) ) ;
#7661 = CIRCLE ( 'NONE', #2862, 1.000000000000000888 ) ;
#7662 = B_SPLINE_CURVE_WITH_KNOTS ( 'NONE', 3,
 ( #2734, #7559, #1621, #8814, #10006, #7877 ),
 .UNSPECIFIED., .F., .F.,
 ( 4, 2, 4 ),
 ( 2.380731630556046949E-07, 0.002336973833157585459, 0.004673709593152115815 ),
 .UNSPECIFIED. ) ;
#7663 = ORIENTED_EDGE ( 'NONE', *, *, #7108, .T. ) ;
#7664 = CARTESIAN_POINT ( 'NONE',  ( 195.1062858801516597, 40.86394065090267702, -219.0000000000000853 ) ) ;
#7665 = DIRECTION ( 'NONE',  ( 3.965082230804130220E-16, 0.000000000000000000, -1.000000000000000000 ) ) ;
#7666 = ADVANCED_FACE ( 'NONE', ( #9911 ), #14700, .T. ) ;
#7667 = CARTESIAN_POINT ( 'NONE',  ( 0.1714848819424952819, 1.330901335694294030, -2.749999999999999556 ) ) ;
#7668 = CARTESIAN_POINT ( 'NONE',  ( -222.1421115826539392, 149.2367494632589455, 7.942719255002825385 ) ) ;
#7669 = ORIENTED_EDGE ( 'NONE', *, *, #4922, .F. ) ;
#7670 = VECTOR ( 'NONE', #12207, 1000.000000000000000 ) ;
#7671 = EDGE_CURVE ( 'NONE', #5101, #4169, #3783, .T. ) ;
#7672 = CARTESIAN_POINT ( 'NONE',  ( -221.4749990704029301, 150.4319862478757273, 9.846583645253028649 ) ) ;
#7673 = ORIENTED_EDGE ( 'NONE', *, *, #6277, .F. ) ;
#7674 = CARTESIAN_POINT ( 'NONE',  ( -170.0824065865490979, 123.5033421008434686, -4.824223088519030256 ) ) ;
#7675 = CARTESIAN_POINT ( 'NONE',  ( 211.8799640061187404, 39.24102814318666788, -4.566144504064119758 ) ) ;
#7677 = ORIENTED_EDGE ( 'NONE', *, *, #338, .T. ) ;
#7676 = AXIS2_PLACEMENT_3D ( 'NONE', #10882, #9615, #8364 ) ;
#7678 = DIRECTION ( 'NONE',  ( -1.000000000000000000, 0.000000000000000000, 0.000000000000000000 ) ) ;
#7679 = DIRECTION ( 'NONE',  ( 0.000000000000000000, -0.1391731009600592484, 0.9902680687415712502 ) ) ;
#7680 = EDGE_CURVE ( 'NONE', #9409, #9433, #562, .T. ) ;
#7681 = DIRECTION ( 'NONE',  ( 1.000000000000000000, 0.000000000000000000, 0.000000000000000000 ) ) ;
#7682 = ORIENTED_EDGE ( 'NONE', *, *, #6218, .F. ) ;
#7683 = AXIS2_PLACEMENT_3D ( 'NONE', #11074, #9657, #9975 ) ;
#7684 = SHAPE_DEFINITION_REPRESENTATION ( #3110, #3298 ) ;
#7685 = ORIENTED_EDGE ( 'NONE', *, *, #1097, .T. ) ;
#7686 = CYLINDRICAL_SURFACE ( 'NONE', #15224, 5.000000000000000000 ) ;
#7687 = CARTESIAN_POINT ( 'NONE',  ( -157.2824335677085799, 110.9804333728871057, 9.692725945294363044 ) ) ;
#7688 = ORIENTED_EDGE ( 'NONE', *, *, #1633, .T. ) ;
#7689 = FACE_OUTER_BOUND ( 'NONE', #8125, .T. ) ;
#7690 = DIRECTION ( 'NONE',  ( 0.000000000000000000, 0.000000000000000000, -1.000000000000000000 ) ) ;
#7691 = VERTEX_POINT ( 'NONE', #13594 ) ;
#7692 = VERTEX_POINT ( 'NONE', #12417 ) ;
#7693 = CARTESIAN_POINT ( 'NONE',  ( -174.7846310273254176, 131.4932641812416421, 2.500000000270498735 ) ) ;
#7694 = CARTESIAN_POINT ( 'NONE',  ( 201.8629198063431716, 32.54887535240757757, -8.146526315903498627 ) ) ;
#7695 = AXIS2_PLACEMENT_3D ( 'NONE', #9142, #12746, #15110 ) ;
#7696 = VERTEX_POINT ( 'NONE', #400 ) ;
#7697 = LINE ( 'NONE', #12560, #10857 ) ;
#7698 = FACE_OUTER_BOUND ( 'NONE', #10538, .T. ) ;
#7699 = CARTESIAN_POINT ( 'NONE',  ( 51.07686401294030532, 368.7106150007013525, 10.00000000000000178 ) ) ;
#7700 = PLANE ( 'NONE',  #3937 ) ;
#7701 = ADVANCED_FACE ( 'NONE', ( #5779 ), #14142, .T. ) ;
#7703 = ADVANCED_FACE ( 'NONE', ( #11714 ), #9347, .F. ) ;
#7702 = ADVANCED_FACE ( 'NONE', ( #9269 ), #3180, .F. ) ;
#7704 = DIRECTION ( 'NONE',  ( -1.000000000000000000, 0.000000000000000000, 0.000000000000000000 ) ) ;
#7705 = ADVANCED_FACE ( 'NONE', ( #8176 ), #13993, .F. ) ;
#7706 = AXIS2_PLACEMENT_3D ( 'NONE', #15261, #11419, #6698 ) ;
#7707 = FACE_OUTER_BOUND ( 'NONE', #309, .T. ) ;
#7708 = ORIENTED_EDGE ( 'NONE', *, *, #4858, .F. ) ;
#7709 = DIRECTION ( 'NONE',  ( -0.000000000000000000, -0.000000000000000000, 1.000000000000000000 ) ) ;
#7710 = CARTESIAN_POINT ( 'NONE',  ( -219.4863873870018267, 149.9206971141745441, -4.874325179114736173 ) ) ;
#7711 = CARTESIAN_POINT ( 'NONE',  ( -212.8881127827856687, 136.6510672405775892, -2.964974570226852624 ) ) ;
#7712 = CARTESIAN_POINT ( 'NONE',  ( 20.93529453487719039, 40.04259805664093363, 10.00000000000000178 ) ) ;
#7713 = ORIENTED_EDGE ( 'NONE', *, *, #2507, .T. ) ;
#7714 = CARTESIAN_POINT ( 'NONE',  ( -221.7331157600676192, 141.5908957077777188, 1.515400478619091551 ) ) ;
#7715 = CARTESIAN_POINT ( 'NONE',  ( 207.1782284445936284, 46.06712597851176838, -2.617760425820522041 ) ) ;
#7716 = VERTEX_POINT ( 'NONE', #5633 ) ;
#7717 = VECTOR ( 'NONE', #3669, 1000.000000000000000 ) ;
#7718 = EDGE_CURVE ( 'NONE', #7692, #6288, #13860, .T. ) ;
#7719 = CARTESIAN_POINT ( 'NONE',  ( 190.5000000000000568, -179.8058001507315566, -30.31842631998718574 ) ) ;
#7720 = CARTESIAN_POINT ( 'NONE',  ( 122.5806775638430253, 45.00321902537314145, 10.00000000000000178 ) ) ;
#7721 = DIRECTION ( 'NONE',  ( 0.000000000000000000, -1.000000000000000000, -4.956352788505160310E-17 ) ) ;
#7722 = EDGE_CURVE ( 'NONE', #9726, #11537, #14064, .T. ) ;
#7723 = CYLINDRICAL_SURFACE ( 'NONE', #14707, 0.5000000000000004441 ) ;
#7724 = ORIENTED_EDGE ( 'NONE', *, *, #1967, .T. ) ;
#7725 = DIRECTION ( 'NONE',  ( 0.000000000000000000, 0.000000000000000000, 1.000000000000000000 ) ) ;
#7726 = AXIS2_PLACEMENT_3D ( 'NONE', #463, #14997, #3167 ) ;
#7727 = CARTESIAN_POINT ( 'NONE',  ( -185.2098801967860595, 137.3018090142982146, 3.478855109513427468 ) ) ;
#7728 = CARTESIAN_POINT ( 'NONE',  ( 177.5000000000000853, -178.9449732516916072, -29.32815825124560760 ) ) ;
#7729 = DIRECTION ( 'NONE',  ( 0.000000000000000000, 0.000000000000000000, -1.000000000000000000 ) ) ;
#7730 = ORIENTED_EDGE ( 'NONE', *, *, #12505, .T. ) ;
#7731 = AXIS2_PLACEMENT_3D ( 'NONE', #6037, #7154, #10699 ) ;
#7732 = FACE_OUTER_BOUND ( 'NONE', #13589, .T. ) ;
#7733 = EDGE_CURVE ( 'NONE', #13786, #7132, #4276, .T. ) ;
#7734 = ORIENTED_EDGE ( 'NONE', *, *, #4024, .F. ) ;
#7735 = ORIENTED_EDGE ( 'NONE', *, *, #2749, .F. ) ;
#7736 = CARTESIAN_POINT ( 'NONE',  ( -63.50000000000002842, 15.53993994372673981, -17.50000000000002487 ) ) ;
#7737 = CARTESIAN_POINT ( 'NONE',  ( 224.0000000000000853, 59.53993994372674337, 25.00000000000000000 ) ) ;
#7738 = FILL_AREA_STYLE ('',( #5121 ) ) ;
#7739 = DIRECTION ( 'NONE',  ( -0.000000000000000000, 1.000000000000000000, -0.000000000000000000 ) ) ;
#7740 = PLANE ( 'NONE',  #4699 ) ;
#7741 = CARTESIAN_POINT ( 'NONE',  ( -217.3145496446415450, 153.8230492215183176, -1.760001856877286608 ) ) ;
#7742 = CIRCLE ( 'NONE', #11766, 3.499999999999999556 ) ;
#7743 = ORIENTED_EDGE ( 'NONE', *, *, #8190, .F. ) ;
#7744 = VECTOR ( 'NONE', #6379, 1000.000000000000000 ) ;
#7745 = LINE ( 'NONE', #7664, #15203 ) ;
#7746 = FACE_OUTER_BOUND ( 'NONE', #15506, .T. ) ;
#7747 = CARTESIAN_POINT ( 'NONE',  ( 207.1325720688761294, 35.61275714886660637, -4.804596322733623914 ) ) ;
#7748 = CARTESIAN_POINT ( 'NONE',  ( -224.4234439893150181, 145.1493843479457553, 0.4584262417508254694 ) ) ;
#7749 = ORIENTED_EDGE ( 'NONE', *, *, #15382, .T. ) ;
#7750 = ADVANCED_FACE ( 'NONE', ( #15163 ), #11548, .F. ) ;
#7751 = CARTESIAN_POINT ( 'NONE',  ( -218.9392864022120193, 154.9751135327425970, 6.220092860173763505 ) ) ;
#7752 = VERTEX_POINT ( 'NONE', #13918 ) ;
#7753 = DIRECTION ( 'NONE',  ( 1.000000000000000000, 0.000000000000000000, 0.000000000000000000 ) ) ;
#7754 = DIRECTION ( 'NONE',  ( 3.965082230804130220E-16, 1.090924371466202084E-47, 1.000000000000000000 ) ) ;
#7755 = ORIENTED_EDGE ( 'NONE', *, *, #9956, .F. ) ;
#7756 = DIRECTION ( 'NONE',  ( 1.000000000000000000, 0.000000000000000000, 0.000000000000000000 ) ) ;
#7757 = DIRECTION ( 'NONE',  ( -1.000000000000000000, 0.000000000000000000, 0.000000000000000000 ) ) ;
#7758 = CARTESIAN_POINT ( 'NONE',  ( 184.0000000000000568, 15.53993994372673626, 48.99999999999997158 ) ) ;
#7759 = ORIENTED_EDGE ( 'NONE', *, *, #2190, .F. ) ;
#7760 = ORIENTED_EDGE ( 'NONE', *, *, #2163, .T. ) ;
#7761 = LINE ( 'NONE', #6345, #6256 ) ;
#7762 = ORIENTED_EDGE ( 'NONE', *, *, #10129, .T. ) ;
#7763 = DIRECTION ( 'NONE',  ( 0.000000000000000000, 0.000000000000000000, 1.000000000000000000 ) ) ;
#7764 = EDGE_CURVE ( 'NONE', #8197, #3561, #10344, .T. ) ;
#7765 = FACE_OUTER_BOUND ( 'NONE', #2404, .T. ) ;
#7766 = EDGE_LOOP ( 'NONE', ( #6250, #14034, #14617, #1663, #7090, #8941, #4738, #10126, #2020 ) ) ;
#7767 = ORIENTED_EDGE ( 'NONE', *, *, #5856, .F. ) ;
#7768 = FACE_OUTER_BOUND ( 'NONE', #2910, .T. ) ;
#7769 = FACE_OUTER_BOUND ( 'NONE', #8226, .T. ) ;
#7770 = ORIENTED_EDGE ( 'NONE', *, *, #10282, .T. ) ;
#7771 = CARTESIAN_POINT ( 'NONE',  ( 205.4081958545874613, 47.87064854543508829, -4.057643371672452481 ) ) ;
#7772 = CARTESIAN_POINT ( 'NONE',  ( 215.4200305399390345, 33.33196348269225240, 5.000000000000000000 ) ) ;
#7773 = DIRECTION ( 'NONE',  ( -3.965082230804130220E-16, 1.090924371466202084E-47, 1.000000000000000000 ) ) ;
#7774 = FACE_OUTER_BOUND ( 'NONE', #14609, .T. ) ;
#7775 = DIRECTION ( 'NONE',  ( 1.000000000000000000, 0.000000000000000000, 0.000000000000000000 ) ) ;
#7776 = PRODUCT_DEFINITION_SHAPE ( 'NONE', 'NONE',  #15627 ) ;
#7777 = EDGE_CURVE ( 'NONE', #2984, #6971, #10083, .T. ) ;
#7778 = VECTOR ( 'NONE', #3775, 1000.000000000000114 ) ;
#7779 = DIRECTION ( 'NONE',  ( 1.000000000000000000, 0.000000000000000000, 0.000000000000000000 ) ) ;
#7780 = AXIS2_PLACEMENT_3D ( 'NONE', #4423, #10671, #15386 ) ;
#7781 = ORIENTED_EDGE ( 'NONE', *, *, #12145, .T. ) ;
#7782 = DIRECTION ( 'NONE',  ( 0.000000000000000000, 0.000000000000000000, -1.000000000000000000 ) ) ;
#7783 = CARTESIAN_POINT ( 'NONE',  ( -63.50000000000002842, 16.03993994372673981, -17.50000000000002487 ) ) ;
#7784 = VECTOR ( 'NONE', #5189, 1000.000000000000000 ) ;
#7785 = ADVANCED_FACE ( 'NONE', ( #15314 ), #2145, .F. ) ;
#7786 = CARTESIAN_POINT ( 'NONE',  ( -211.2943419521749888, 151.8811774793218490, 1.515441477536285220 ) ) ;
#7788 = CARTESIAN_POINT ( 'NONE',  ( 70.26535645333922275, 38.79159067395544014, 10.00000000000000178 ) ) ;
#7787 = PRODUCT_RELATED_PRODUCT_CATEGORY ( 'part', '', ( #13944 ) ) ;
#7789 = VERTEX_POINT ( 'NONE', #10605 ) ;
#7790 = CARTESIAN_POINT ( 'NONE',  ( -183.9313806081839289, 121.1548445249323720, 7.918248976830652097 ) ) ;
#7791 = CARTESIAN_POINT ( 'NONE',  ( 198.3913412372077687, 29.09831693401786268, -0.7477385443502184703 ) ) ;
#7792 = ORIENTED_EDGE ( 'NONE', *, *, #12403, .F. ) ;
#7793 = EDGE_CURVE ( 'NONE', #14616, #14639, #10293, .T. ) ;
#7794 = VECTOR ( 'NONE', #13985, 1000.000000000000000 ) ;
#7795 = DIRECTION ( 'NONE',  ( 1.000000000000000000, 0.000000000000000000, 0.000000000000000000 ) ) ;
#7796 = CARTESIAN_POINT ( 'NONE',  ( 177.5000000000000853, 16.03993994372673981, 25.38206912977649665 ) ) ;
#7797 = CARTESIAN_POINT ( 'NONE',  ( -85.99999999999994316, 64.53993994372673626, 15.00000000000174794 ) ) ;
#7798 = AXIS2_PLACEMENT_3D ( 'NONE', #1371, #2489, #4941 ) ;
#7799 = CARTESIAN_POINT ( 'NONE',  ( 190.0000000000000853, -179.3058001507315566, 65.31842631998698323 ) ) ;
#7800 = VERTEX_POINT ( 'NONE', #6825 ) ;
#7801 = DIRECTION ( 'NONE',  ( 2.751328491981765035E-32, -1.000000000000000000, -1.090924371466202084E-47 ) ) ;
#7802 = EDGE_CURVE ( 'NONE', #14996, #5691, #1247, .T. ) ;
#7803 = EDGE_CURVE ( 'NONE', #12658, #138, #11637, .T. ) ;
#7804 = EDGE_CURVE ( 'NONE', #13575, #592, #12853, .T. ) ;
#7805 = CARTESIAN_POINT ( 'NONE',  ( -205.6684400016210645, 139.7560197894119085, 10.16010209732751157 ) ) ;
#7806 = AXIS2_PLACEMENT_3D ( 'NONE', #3999, #10094, #7654 ) ;
#7807 = CARTESIAN_POINT ( 'NONE',  ( 0.000000000000000000, 0.000000000000000000, 0.000000000000000000 ) ) ;
#7808 = AXIS2_PLACEMENT_3D ( 'NONE', #1956, #6794, #3002 ) ;
#7809 = DIRECTION ( 'NONE',  ( -0.000000000000000000, 1.000000000000000000, 1.156482317317871725E-16 ) ) ;
#7810 = ORIENTED_EDGE ( 'NONE', *, *, #14425, .T. ) ;
#7811 = DIRECTION ( 'NONE',  ( -3.965082230804130220E-16, 0.000000000000000000, -1.000000000000000000 ) ) ;
#7812 = AXIS2_PLACEMENT_3D ( 'NONE', #9105, #13906, #5303 ) ;
#7813 = ORIENTED_EDGE ( 'NONE', *, *, #3332, .T. ) ;
#7814 = ORIENTED_EDGE ( 'NONE', *, *, #7804, .T. ) ;
#7815 = FACE_OUTER_BOUND ( 'NONE', #11963, .T. ) ;
#7816 = CARTESIAN_POINT ( 'NONE',  ( 5.196152422706635576, -9.000000000000003553, 0.000000000000000000 ) ) ;
#7817 = CARTESIAN_POINT ( 'NONE',  ( 2.000000000000000000, -1.587713240271472648, -2.750000000000000888 ) ) ;
#7818 = CARTESIAN_POINT ( 'NONE',  ( -76.00000000000001421, -178.8058001507315566, -30.31842631998718574 ) ) ;
#7819 = CARTESIAN_POINT ( 'NONE',  ( -218.9290471127720821, 154.9934588271201505, -1.343261102213330949 ) ) ;
#7820 = AXIS2_PLACEMENT_3D ( 'NONE', #8113, #12898, #891 ) ;
#7821 = CARTESIAN_POINT ( 'NONE',  ( -155.6477983077465410, 110.1970436846185066, 5.000000000000000000 ) ) ;
#7822 = AXIS2_PLACEMENT_3D ( 'NONE', #11777, #3170, #9408 ) ;
#7823 = EDGE_CURVE ( 'NONE', #5068, #6329, #10451, .T. ) ;
#7824 = DIRECTION ( 'NONE',  ( 0.000000000000000000, 0.000000000000000000, -1.000000000000000000 ) ) ;
#7825 = CARTESIAN_POINT ( 'NONE',  ( 51.39999999999999858, 5.109226446042775356E-16, -4.172000000000013920 ) ) ;
#7826 = CARTESIAN_POINT ( 'NONE',  ( 193.1007612367029367, 46.15997280778478995, -6.307360761128419036 ) ) ;
#7827 = CONICAL_SURFACE ( 'NONE', #14100, 2.749999999999999112, 1.047197551196600296 ) ;
#7828 = CARTESIAN_POINT ( 'NONE',  ( 184.0000000000000568, 17.53993994372673271, 47.49999999999997868 ) ) ;
#7829 = ORIENTED_EDGE ( 'NONE', *, *, #4992, .T. ) ;
#7830 = AXIS2_PLACEMENT_3D ( 'NONE', #5404, #15015, #13678 ) ;
#7831 = VECTOR ( 'NONE', #559, 1000.000000000000114 ) ;
#7832 = CARTESIAN_POINT ( 'NONE',  ( -219.0004266419835801, 154.8655711957941890, 6.428065963712064956 ) ) ;
#7833 = ORIENTED_EDGE ( 'NONE', *, *, #8001, .F. ) ;
#7834 = FACE_OUTER_BOUND ( 'NONE', #5239, .T. ) ;
#7835 = DIRECTION ( 'NONE',  ( 0.000000000000000000, 0.000000000000000000, -1.000000000000000000 ) ) ;
#7836 = AXIS2_PLACEMENT_3D ( 'NONE', #6598, #1522, #11172 ) ;
#7837 = ORIENTED_EDGE ( 'NONE', *, *, #4858, .T. ) ;
#7838 = CARTESIAN_POINT ( 'NONE',  ( -157.6477983077465694, 110.1970436846185066, 84.88378295107887084 ) ) ;
#7839 = DIRECTION ( 'NONE',  ( 0.000000000000000000, 0.000000000000000000, 1.000000000000000000 ) ) ;
#7840 = ADVANCED_FACE ( 'NONE', ( #4916 ), #8406, .T. ) ;
#7841 = VECTOR ( 'NONE', #2876, 1000.000000000000000 ) ;
#7842 = CARTESIAN_POINT ( 'NONE',  ( 5.799999999999999822, 7.999999999999979572, 0.000000000000000000 ) ) ;
#7843 = ORIENTED_EDGE ( 'NONE', *, *, #6986, .F. ) ;
#7844 = AXIS2_PLACEMENT_3D ( 'NONE', #15133, #14107, #4324 ) ;
#7845 = ORIENTED_EDGE ( 'NONE', *, *, #6120, .T. ) ;
#7846 = CARTESIAN_POINT ( 'NONE',  ( 193.0454511798755846, 35.63895119138042133, -1.116400838283317043 ) ) ;
#7847 = FACE_OUTER_BOUND ( 'NONE', #3242, .T. ) ;
#7848 = ORIENTED_EDGE ( 'NONE', *, *, #3820, .F. ) ;
#7849 = LINE ( 'NONE', #12636, #2147 ) ;
#7850 = DIRECTION ( 'NONE',  ( 0.000000000000000000, 0.000000000000000000, -1.000000000000000000 ) ) ;
#7851 = AXIS2_PLACEMENT_3D ( 'NONE', #10038, #5375, #3006 ) ;
#7852 = ORIENTED_EDGE ( 'NONE', *, *, #4595, .F. ) ;
#7853 = ORIENTED_EDGE ( 'NONE', *, *, #2189, .F. ) ;
#7854 = CARTESIAN_POINT ( 'NONE',  ( -206.8718859864436581, 149.4025266312245037, 2.500000000000000000 ) ) ;
#7855 = CARTESIAN_POINT ( 'NONE',  ( -85.27455057502459113, 65.19100426474074084, 5.000000000000000000 ) ) ;
#7856 = AXIS2_PLACEMENT_3D ( 'NONE', #2830, #12368, #7651 ) ;
#7857 = ORIENTED_EDGE ( 'NONE', *, *, #9621, .F. ) ;
#7859 = EDGE_CURVE ( 'NONE', #5720, #10088, #3644, .T. ) ;
#7858 = CARTESIAN_POINT ( 'NONE',  ( 191.3844089520862894, 42.02011290432638901, -3.056456915890917170 ) ) ;
#7860 = CARTESIAN_POINT ( 'NONE',  ( 14.00000000000004086, 64.53993994372673626, 15.00000000000104983 ) ) ;
#7861 = DIRECTION ( 'NONE',  ( 3.965082230804130220E-16, 0.000000000000000000, -1.000000000000000000 ) ) ;
#7862 = CARTESIAN_POINT ( 'NONE',  ( 19.11029453487719110, 40.04259805664093363, 7.600000000000002309 ) ) ;
#7863 = EDGE_CURVE ( 'NONE', #10197, #701, #13164, .T. ) ;
#7864 = DIRECTION ( 'NONE',  ( 0.000000000000000000, 0.000000000000000000, -1.000000000000000000 ) ) ;
#7865 = DIRECTION ( 'NONE',  ( -0.3662838836490107108, 0.9305003370641705684, 0.002288952263120965468 ) ) ;
#7866 = VECTOR ( 'NONE', #8917, 1000.000000000000000 ) ;
#7867 = ORIENTED_EDGE ( 'NONE', *, *, #5084, .F. ) ;
#7868 = EDGE_CURVE ( 'NONE', #6130, #9708, #77, .T. ) ;
#7869 = CARTESIAN_POINT ( 'NONE',  ( -110.0000000000000426, 56.53993994372675047, 13.00000000000000178 ) ) ;
#7870 = CARTESIAN_POINT ( 'NONE',  ( -182.2196890910978482, 130.3369809632412739, -4.640918829492416187 ) ) ;
#7871 = DIRECTION ( 'NONE',  ( 0.000000000000000000, -1.000000000000000000, -1.156482317317871725E-16 ) ) ;
#7872 = VERTEX_POINT ( 'NONE', #6103 ) ;
#7873 = CARTESIAN_POINT ( 'NONE',  ( -221.5559209476002991, 141.9078401207188449, -0.4555467707853290138 ) ) ;
#7874 = CARTESIAN_POINT ( 'NONE',  ( 203.2625657313046190, 29.78760669494945645, -9.693656633365744568 ) ) ;
#7875 = ORIENTED_EDGE ( 'NONE', *, *, #1861, .T. ) ;
#7876 = VECTOR ( 'NONE', #10675, 1000.000000000000000 ) ;
#7877 = CARTESIAN_POINT ( 'NONE',  ( 0.000000000000000000, -6.928203230275514990, -4.000000000000003553 ) ) ;
#7878 = CARTESIAN_POINT ( 'NONE',  ( -61.94838851346079167, -178.8058001507315566, 65.31842631998698323 ) ) ;
#7879 =( REPRESENTATION_RELATIONSHIP ('NONE','NONE', #3298, #11876 ) REPRESENTATION_RELATIONSHIP_WITH_TRANSFORMATION ( #2208 )SHAPE_REPRESENTATION_RELATIONSHIP( ) );
#7880 = FACE_OUTER_BOUND ( 'NONE', #4425, .T. ) ;
#7881 = EDGE_CURVE ( 'NONE', #8586, #1592, #14675, .T. ) ;
#7882 = CARTESIAN_POINT ( 'NONE',  ( -108.0000000000000568, 26.39124795404934076, 0.000000000000000000 ) ) ;
#7883 = ORIENTED_EDGE ( 'NONE', *, *, #715, .F. ) ;
#7884 = AXIS2_PLACEMENT_3D ( 'NONE', #7506, #10029, #5281 ) ;
#7885 = CARTESIAN_POINT ( 'NONE',  ( -63.50000000000002842, 16.03993994372673981, -3.075184203610571654 ) ) ;
#7886 = CARTESIAN_POINT ( 'NONE',  ( -210.8662606591548752, 142.3010704693858486, 10.16010209732750624 ) ) ;
#7887 = CARTESIAN_POINT ( 'NONE',  ( -63.50000000000002842, 17.53993994372674692, -17.50000000000002487 ) ) ;
#7888 = CIRCLE ( 'NONE', #10386, 1.000000000000000888 ) ;
#7889 = CARTESIAN_POINT ( 'NONE',  ( -157.4608918519057568, 110.7933268109660787, -4.760088435541717011 ) ) ;
#7890 = EDGE_LOOP ( 'NONE', ( #7941, #8523, #11641, #527 ) ) ;
#7891 = CARTESIAN_POINT ( 'NONE',  ( -110.0000000000000426, 22.53993994372673981, 13.00000000000000178 ) ) ;
#7892 = ORIENTED_EDGE ( 'NONE', *, *, #14841, .T. ) ;
#7893 = ORIENTED_EDGE ( 'NONE', *, *, #8236, .T. ) ;
#7894 = CARTESIAN_POINT ( 'NONE',  ( -83.57455057502457407, 65.19100426474074084, 5.000000000000000000 ) ) ;
#7895 = CARTESIAN_POINT ( 'NONE',  ( -70.00000000000000000, 17.53993994372673271, 48.99999999999997158 ) ) ;
#7896 = SURFACE_STYLE_USAGE ( .BOTH. , #4233 ) ;
#7897 = CARTESIAN_POINT ( 'NONE',  ( -167.8991350591905416, 127.4150157579244080, 4.345048324134917372 ) ) ;
#7898 = CARTESIAN_POINT ( 'NONE',  ( -216.7281194157721131, 154.8360440772405866, 1.364217605950574397 ) ) ;
#7899 = EDGE_CURVE ( 'NONE', #10985, #14187, #8905, .T. ) ;
#7901 = ADVANCED_FACE ( 'NONE', ( #13340 ), #147, .T. ) ;
#7900 = EDGE_CURVE ( 'NONE', #14639, #8637, #1039, .T. ) ;
#7902 = LINE ( 'NONE', #6555, #6968 ) ;
#7904 = CLOSED_SHELL ( 'NONE', ( #3239, #5508, #1273, #2565, #8100, #3035, #5550, #15025, #7129, #6885, #12985, #13603, #8014, #1217, #4429, #1016, #7931, #4201, #2473 ) ) ;
#7903 = AXIS2_PLACEMENT_3D ( 'NONE', #798, #9117, #5558 ) ;
#7905 = CARTESIAN_POINT ( 'NONE',  ( 14.00000000000004086, 59.53993994372674337, 15.00000000000104983 ) ) ;
#7906 = CARTESIAN_POINT ( 'NONE',  ( 177.5000000000000853, 15.60952649420677041, 9.122796835852554409 ) ) ;
#7907 = CARTESIAN_POINT ( 'NONE',  ( 178.0000000000000853, -178.8058001507315566, -17.19066787724516843 ) ) ;
#7908 = CARTESIAN_POINT ( 'NONE',  ( -220.0724991394543224, 152.9447850296022864, -1.223998976589070864 ) ) ;
#7909 = ORIENTED_EDGE ( 'NONE', *, *, #2766, .F. ) ;
#7910 = ORIENTED_EDGE ( 'NONE', *, *, #2682, .T. ) ;
#7911 = CARTESIAN_POINT ( 'NONE',  ( -151.4086188282879277, 107.2728346664360259, 0.000000000000000000 ) ) ;
#7912 = CARTESIAN_POINT ( 'NONE',  ( -63.50000000000002842, -179.8058001507315566, -17.19066787724516843 ) ) ;
#7913 = ORIENTED_EDGE ( 'NONE', *, *, #8029, .T. ) ;
#7914 = DIRECTION ( 'NONE',  ( -1.000000000000000000, -0.000000000000000000, -0.000000000000000000 ) ) ;
#7915 = DIRECTION ( 'NONE',  ( -0.000000000000000000, 1.000000000000000000, 6.938893903907227145E-17 ) ) ;
#7916 = PRODUCT ( 'Handle Balance Weight Counterbalance', 'Handle Balance Weight Counterbalance', '', ( #6257 ) ) ;
#7917 = CARTESIAN_POINT ( 'NONE',  ( 0.000000000000000000, 0.000000000000000000, 0.000000000000000000 ) ) ;
#7918 = EDGE_LOOP ( 'NONE', ( #10780, #13723, #12286, #1030 ) ) ;
#7919 = APPLICATION_PROTOCOL_DEFINITION ( 'draft international standard', 'automotive_design', 1998, #5649 ) ;
#7920 = ORIENTED_EDGE ( 'NONE', *, *, #8481, .F. ) ;
#7921 = AXIS2_PLACEMENT_3D ( 'NONE', #11210, #10028, #5128 ) ;
#7922 = CARTESIAN_POINT ( 'NONE',  ( 211.9100270530500154, 42.38063601863193242, 0.1257832527464326222 ) ) ;
#7923 = DIRECTION ( 'NONE',  ( 0.000000000000000000, 0.000000000000000000, 1.000000000000000000 ) ) ;
#7924 = VERTEX_POINT ( 'NONE', #7137 ) ;
#7925 = DIRECTION ( 'NONE',  ( -1.000000000000000000, -0.000000000000000000, -0.000000000000000000 ) ) ;
#7926 = B_SPLINE_CURVE_WITH_KNOTS ( 'NONE', 3,
 ( #3613, #1158, #12135, #1315, #10805, #6071, #2590, #9537, #10964, #2271, #4800, #8448, #13228, #2428, #7260, #8518 ),
 .UNSPECIFIED., .F., .F.,
 ( 4, 2, 2, 2, 2, 2, 2, 4 ),
 ( 1.430489624538199204E-17, 0.0004036473355434303683, 0.0008072946710868464252, 0.001210942006630262536, 0.001614589342173678539, 0.002421884013260430530, 0.002825531348803793190, 0.003229178684347155416 ),
 .UNSPECIFIED. ) ;
#7927 = DIRECTION ( 'NONE',  ( 1.000000000000000000, 0.000000000000000000, 0.000000000000000000 ) ) ;
#7928 = ORIENTED_EDGE ( 'NONE', *, *, #72, .F. ) ;
#7929 = ORIENTED_EDGE ( 'NONE', *, *, #3059, .F. ) ;
#7930 = DIRECTION ( 'NONE',  ( -1.000000000000000000, 0.000000000000000000, 0.000000000000000000 ) ) ;
#7931 = ADVANCED_FACE ( 'NONE', ( #1113 ), #9405, .T. ) ;
#7932 = ORIENTED_EDGE ( 'NONE', *, *, #1908, .T. ) ;
#7933 = CARTESIAN_POINT ( 'NONE',  ( 207.1325720688761294, 35.61275714886660637, -4.804596322733623914 ) ) ;
#7934 = DIRECTION ( 'NONE',  ( 0.8731965799097685110, -0.4873681696970816324, -0.000000000000000000 ) ) ;
#7935 = AXIS2_PLACEMENT_3D ( 'NONE', #12614, #9002, #13718 ) ;
#7936 = CARTESIAN_POINT ( 'NONE',  ( 0.000000000000000000, 0.000000000000000000, 0.000000000000000000 ) ) ;
#7937 = PLANE ( 'NONE',  #5456 ) ;
#7938 = DIRECTION ( 'NONE',  ( -0.000000000000000000, -0.000000000000000000, -1.000000000000000000 ) ) ;
#7939 = CIRCLE ( 'NONE', #1104, 1.700000000000007061 ) ;
#7940 = DIRECTION ( 'NONE',  ( 0.000000000000000000, -0.000000000000000000, -1.000000000000000000 ) ) ;
#7941 = ORIENTED_EDGE ( 'NONE', *, *, #7416, .F. ) ;
#7942 = CARTESIAN_POINT ( 'NONE',  ( 163.3793289068652257, 15.80605437029538507, -6.370175303308196924 ) ) ;
#7943 = CIRCLE ( 'NONE', #11965, 1.000000000000000888 ) ;
#7944 = CARTESIAN_POINT ( 'NONE',  ( -185.2011473888584874, 137.3174552105199666, 1.515441477536283887 ) ) ;
#7945 = DIRECTION ( 'NONE',  ( 0.000000000000000000, 0.000000000000000000, 1.000000000000000000 ) ) ;
#7946 = ORIENTED_EDGE ( 'NONE', *, *, #7021, .T. ) ;
#7947 = ADVANCED_FACE ( 'NONE', ( #7372 ), #12165, .F. ) ;
#7948 = CARTESIAN_POINT ( 'NONE',  ( -193.5420962672365022, 128.8371742780315969, -2.964974570226833084 ) ) ;
#7949 = CARTESIAN_POINT ( 'NONE',  ( 207.4107378919655673, 50.26574450011962369, -5.500654858001599479 ) ) ;
#7950 = EDGE_LOOP ( 'NONE', ( #3844, #11036, #11992, #11774 ) ) ;
#7951 = CARTESIAN_POINT ( 'NONE',  ( -64.00000000000002842, 15.17911304468680100, 9.062306170389884841 ) ) ;
#7952 = DIRECTION ( 'NONE',  ( -0.000000000000000000, -0.000000000000000000, 1.000000000000000000 ) ) ;
#7953 = EDGE_CURVE ( 'NONE', #11614, #10036, #2225, .T. ) ;
#7954 = CARTESIAN_POINT ( 'NONE',  ( -150.4086188282879277, 107.1404563131855809, -4.828669606760403354 ) ) ;
#7955 = AXIS2_PLACEMENT_3D ( 'NONE', #9289, #9370, #3056 ) ;
#7956 = PLANE ( 'NONE',  #9141 ) ;
#7957 = ORIENTED_EDGE ( 'NONE', *, *, #13818, .F. ) ;
#7958 = DIRECTION ( 'NONE',  ( -0.000000000000000000, -0.000000000000000000, 1.000000000000000000 ) ) ;
#7959 = CARTESIAN_POINT ( 'NONE',  ( -198.9139648670198994, 132.3922632189928095, 9.577123744044227394 ) ) ;
#7960 = CARTESIAN_POINT ( 'NONE',  ( -70.00000000000000000, 15.53993994372673981, -12.49999999999999289 ) ) ;
#7961 = CARTESIAN_POINT ( 'NONE',  ( 172.0899380277727744, 70.88000906936352408, -0.9107274384406883749 ) ) ;
#7962 = VERTEX_POINT ( 'NONE', #14604 ) ;
#7963 = DIRECTION ( 'NONE',  ( 1.000000000000000000, 0.000000000000000000, 0.000000000000000000 ) ) ;
#7964 = CIRCLE ( 'NONE', #2909, 1.500000000000000666 ) ;
#7965 = EDGE_CURVE ( 'NONE', #5664, #2142, #3807, .T. ) ;
#7966 = ORIENTED_EDGE ( 'NONE', *, *, #11533, .T. ) ;
#7967 = ORIENTED_EDGE ( 'NONE', *, *, #12504, .T. ) ;
#7968 = DIRECTION ( 'NONE',  ( 0.000000000000000000, -0.1391731009600592484, 0.9902680687415712502 ) ) ;
#7969 = FACE_BOUND ( 'NONE', #2278, .T. ) ;
#7970 = LINE ( 'NONE', #4394, #6148 ) ;
#7971 = CARTESIAN_POINT ( 'NONE',  ( -170.2135745989010047, 123.2683340168104422, 9.619678501396277781 ) ) ;
#7972 = CARTESIAN_POINT ( 'NONE',  ( -219.2752461992650979, 150.3093291563185687, -4.757798792355696804 ) ) ;
#7973 = DIRECTION ( 'NONE',  ( -0.000000000000000000, -1.000000000000000000, -0.000000000000000000 ) ) ;
#7974 = VECTOR ( 'NONE', #4996, 1000.000000000000000 ) ;
#7975 = CYLINDRICAL_SURFACE ( 'NONE', #6661, 0.5000000000000004441 ) ;
#7976 = FACE_OUTER_BOUND ( 'NONE', #8748, .T. ) ;
#7977 = VECTOR ( 'NONE', #9053, 1000.000000000000227 ) ;
#7978 = ADVANCED_FACE ( 'NONE', ( #9654 ), #8625, .F. ) ;
#7979 = CARTESIAN_POINT ( 'NONE',  ( 200.1062858801516597, 40.86394065090267702, 16.00000000000001421 ) ) ;
#7980 = FACE_OUTER_BOUND ( 'NONE', #3654, .T. ) ;
#7981 = CARTESIAN_POINT ( 'NONE',  ( -223.0548572358123067, 147.6014223487273682, -2.597100425689188086 ) ) ;
#7982 = VERTEX_POINT ( 'NONE', #15475 ) ;
#7983 = ADVANCED_FACE ( 'NONE', ( #4669 ), #4747, .F. ) ;
#7984 = VERTEX_POINT ( 'NONE', #8324 ) ;
#7985 = EDGE_CURVE ( 'NONE', #6589, #5209, #13109, .T. ) ;
#7986 = CARTESIAN_POINT ( 'NONE',  ( -76.50000000000001421, -179.8058001507315566, 84.88378295107887084 ) ) ;
#7987 = DIRECTION ( 'NONE',  ( 0.000000000000000000, -0.000000000000000000, 1.000000000000000000 ) ) ;
#7988 = DIRECTION ( 'NONE',  ( 3.965082230804130220E-16, 4.956352788505162775E-17, -1.000000000000000000 ) ) ;
#7989 = CARTESIAN_POINT ( 'NONE',  ( 200.1062858801516597, 33.86394065090269123, 12.00000000000001066 ) ) ;
#7990 = DIRECTION ( 'NONE',  ( 0.000000000000000000, -1.000000000000000000, 0.000000000000000000 ) ) ;
#7991 = EDGE_CURVE ( 'NONE', #9297, #10399, #2601, .T. ) ;
#7992 = AXIS2_PLACEMENT_3D ( 'NONE', #9695, #1153, #9531 ) ;
#7993 = DIRECTION ( 'NONE',  ( -1.000000000000000000, 0.000000000000000000, 0.000000000000000000 ) ) ;
#7994 = ORIENTED_EDGE ( 'NONE', *, *, #9954, .F. ) ;
#7995 = SHAPE_DEFINITION_REPRESENTATION ( #3232, #3806 ) ;
#7996 = VERTEX_POINT ( 'NONE', #378 ) ;
#7997 = CARTESIAN_POINT ( 'NONE',  ( 192.9390872975532716, 31.37216231216662266, -4.138271986312449080 ) ) ;
#7998 = ORIENTED_EDGE ( 'NONE', *, *, #916, .F. ) ;
#7999 = AXIS2_PLACEMENT_3D ( 'NONE', #11843, #6160, #7115 ) ;
#8000 = DIRECTION ( 'NONE',  ( 1.000000000000000000, 0.000000000000000000, 0.000000000000000000 ) ) ;
#8001 = EDGE_CURVE ( 'NONE', #12589, #4389, #1737, .T. ) ;
#8002 = EDGE_CURVE ( 'NONE', #6470, #12466, #9892, .T. ) ;
#8003 = CARTESIAN_POINT ( 'NONE',  ( -163.5604377276969217, 108.5145932403815721, 0.000000000000000000 ) ) ;
#8004 = VERTEX_POINT ( 'NONE', #5219 ) ;
#8005 = ORIENTED_EDGE ( 'NONE', *, *, #12091, .T. ) ;
#8006 = CARTESIAN_POINT ( 'NONE',  ( -174.2824251065520968, 115.9783496305641535, 2.177446462082195389 ) ) ;
#8007 = CARTESIAN_POINT ( 'NONE',  ( -223.5918188539070002, 142.0538562971642307, 1.612306317632525854 ) ) ;
#8008 = ORIENTED_EDGE ( 'NONE', *, *, #4797, .F. ) ;
#8009 = LINE ( 'NONE', #6511, #14112 ) ;
#8010 = DIRECTION ( 'NONE',  ( -0.000000000000000000, 1.000000000000000000, -0.000000000000000000 ) ) ;
#8011 = FACE_OUTER_BOUND ( 'NONE', #7645, .T. ) ;
#8012 = LINE ( 'NONE', #4434, #11258 ) ;
#8013 = DIRECTION ( 'NONE',  ( 0.000000000000000000, -1.000000000000000000, -6.938893903907227145E-17 ) ) ;
#8014 = ADVANCED_FACE ( 'NONE', ( #11294 ), #15424, .T. ) ;
#8015 = DIRECTION ( 'NONE',  ( -1.000000000000000000, 0.000000000000000000, 0.000000000000000000 ) ) ;
#8016 = VERTEX_POINT ( 'NONE', #12240 ) ;
#8017 = CYLINDRICAL_SURFACE ( 'NONE', #6454, 1.700000000000007061 ) ;
#8018 = CARTESIAN_POINT ( 'NONE',  ( -174.4670243326416994, 126.3579851466298010, -4.682492215613329734 ) ) ;
#8019 = DIRECTION ( 'NONE',  ( -0.3297523322010256219, -0.9440639390088612082, 0.002584273796984222320 ) ) ;
#8020 = ORIENTED_EDGE ( 'NONE', *, *, #10058, .F. ) ;
#8021 = CARTESIAN_POINT ( 'NONE',  ( -205.6342130761154863, 139.8173426991758959, -5.230826428279590878 ) ) ;
#8022 = UNCERTAINTY_MEASURE_WITH_UNIT (LENGTH_MEASURE( 1.000000000000000082E-05 ), #12007, 'distance_accuracy_value', 'NONE');
#8023 = CARTESIAN_POINT ( 'NONE',  ( 201.7245916543302826, 29.07256658421868423, -6.764440628860102223 ) ) ;
#8024 = ORIENTED_EDGE ( 'NONE', *, *, #12016, .F. ) ;
#8025 = CARTESIAN_POINT ( 'NONE',  ( -76.50000000000001421, -178.8753867012115961, 64.82329228561619061 ) ) ;
#8026 = CARTESIAN_POINT ( 'NONE',  ( 0.02311621069251519611, -0.5352285650591098731, 2.749999999999999112 ) ) ;
#8027 = CYLINDRICAL_SURFACE ( 'NONE', #2542, 9.999999999999994671 ) ;
#8028 = VECTOR ( 'NONE', #281, 999.9999999999998863 ) ;
#8029 = EDGE_CURVE ( 'NONE', #5720, #10245, #2620, .T. ) ;
#8030 = ORIENTED_EDGE ( 'NONE', *, *, #11962, .F. ) ;
#8031 = AXIS2_PLACEMENT_3D ( 'NONE', #2901, #6537, #8803 ) ;
#8032 =( NAMED_UNIT ( * ) PLANE_ANGLE_UNIT ( ) SI_UNIT ( $, .RADIAN. ) );
#8033 = CARTESIAN_POINT ( 'NONE',  ( 164.0000000000000568, 64.53993994372673626, 11.47500000000000320 ) ) ;
#8034 = EDGE_CURVE ( 'NONE', #5037, #15478, #14830, .T. ) ;
#8035 = ORIENTED_EDGE ( 'NONE', *, *, #14813, .T. ) ;
#8036 = DIRECTION ( 'NONE',  ( 0.000000000000000000, -0.1391731009600591096, 0.9902680687415711391 ) ) ;
#8037 = CARTESIAN_POINT ( 'NONE',  ( -196.0016709267559349, 137.8086561579936813, 9.578254705571842109 ) ) ;
#8038 = DIRECTION ( 'NONE',  ( 1.000000000000000000, 0.000000000000000000, 0.000000000000000000 ) ) ;
#8039 = CARTESIAN_POINT ( 'NONE',  ( 0.000000000000000000, 15.03993994372673981, 10.05257423913146475 ) ) ;
#8040 = PRODUCT ( 'Handle Grip', 'Handle Grip', '', ( #8864 ) ) ;
#8041 = ORIENTED_EDGE ( 'NONE', *, *, #4864, .F. ) ;
#8042 = FACE_OUTER_BOUND ( 'NONE', #787, .T. ) ;
#8043 = AXIS2_PLACEMENT_3D ( 'NONE', #2060, #10599, #8170 ) ;
#8044 = ORIENTED_EDGE ( 'NONE', *, *, #14903, .F. ) ;
#8045 = EDGE_LOOP ( 'NONE', ( #10510, #7957, #13280, #143 ) ) ;
#8046 = DIRECTION ( 'NONE',  ( 1.000000000000000000, 0.000000000000000000, 0.000000000000000000 ) ) ;
#8047 = DIRECTION ( 'NONE',  ( -0.000000000000000000, -0.9902680687415710281, 0.1391731009600611635 ) ) ;
#8048 = AXIS2_PLACEMENT_3D ( 'NONE', #1502, #11964, #5069 ) ;
#8049 = CIRCLE ( 'NONE', #1713, 3.500000000000003109 ) ;
#8050 = DIRECTION ( 'NONE',  ( -0.000000000000000000, -0.000000000000000000, 1.000000000000000000 ) ) ;
#8051 = CARTESIAN_POINT ( 'NONE',  ( -171.5607450841399384, 120.8546666224106048, 9.733687684402502427 ) ) ;
#8052 = CARTESIAN_POINT ( 'NONE',  ( -222.8126188176429991, 148.0354304998946589, -2.784116551314819610 ) ) ;
#8053 = CARTESIAN_POINT ( 'NONE',  ( 178.0000000000000853, -178.8058001507315566, 52.19066787724494816 ) ) ;
#8054 = VECTOR ( 'NONE', #7049, 1000.000000000000000 ) ;
#8055 = FACE_OUTER_BOUND ( 'NONE', #12520, .T. ) ;
#8056 = AXIS2_PLACEMENT_3D ( 'NONE', #15494, #11808, #1927 ) ;
#8057 = EDGE_CURVE ( 'NONE', #12734, #10742, #8644, .T. ) ;
#8058 = DIRECTION ( 'NONE',  ( -0.000000000000000000, 0.000000000000000000, 1.000000000000000000 ) ) ;
#8059 = CIRCLE ( 'NONE', #12558, 1.700000000000007061 ) ;
#8060 = CARTESIAN_POINT ( 'NONE',  ( -224.5272311398514091, 144.9634333759256322, 1.130582765413566282 ) ) ;
#8061 = VERTEX_POINT ( 'NONE', #6495 ) ;
#8062 =( NAMED_UNIT ( * ) PLANE_ANGLE_UNIT ( ) SI_UNIT ( $, .RADIAN. ) );
#8063 = ORIENTED_EDGE ( 'NONE', *, *, #5038, .T. ) ;
#8064 = FACE_OUTER_BOUND ( 'NONE', #466, .T. ) ;
#8065 = CARTESIAN_POINT ( 'NONE',  ( 14.00000000000004086, 56.53993994372675047, 16.70000000000105089 ) ) ;
#8066 = DIRECTION ( 'NONE',  ( 0.000000000000000000, 0.000000000000000000, -1.000000000000000000 ) ) ;
#8067 = CIRCLE ( 'NONE', #14088, 1.499999999999994449 ) ;
#8068 = CARTESIAN_POINT ( 'NONE',  ( 190.0000000000000568, 15.03993994372673981, 10.05257423913146475 ) ) ;
#8069 = DIRECTION ( 'NONE',  ( 0.000000000000000000, -3.469446951953611033E-15, 1.000000000000000000 ) ) ;
#8070 = CIRCLE ( 'NONE', #13344, 1.700000000000007061 ) ;
#8071 = AXIS2_PLACEMENT_3D ( 'NONE', #7, #8713, #2466 ) ;
#8072 = CARTESIAN_POINT ( 'NONE',  ( 176.0543059057019661, 61.25683321636181233, 10.00000000000000178 ) ) ;
#8073 = VERTEX_POINT ( 'NONE', #6338 ) ;
#8074 = ADVANCED_FACE ( 'NONE', ( #540 ), #10409, .F. ) ;
#8075 = VECTOR ( 'NONE', #9380, 1000.000000000000000 ) ;
#8076 = CONTEXT_DEPENDENT_SHAPE_REPRESENTATION ( #13700, #7776 ) ;
#8077 = CIRCLE ( 'NONE', #6048, 1.700000000000007061 ) ;
#8078 = EDGE_LOOP ( 'NONE', ( #11298, #6849 ) ) ;
#8079 = VECTOR ( 'NONE', #3702, 1000.000000000000000 ) ;
#8080 = CARTESIAN_POINT ( 'NONE',  ( 209.5435894037482285, 33.63601521402413397, -0.2471466635189603911 ) ) ;
#8081 = CARTESIAN_POINT ( 'NONE',  ( -5.196152422706630247, -9.000000000000005329, 5.000000000000000000 ) ) ;
#8082 = VERTEX_POINT ( 'NONE', #7758 ) ;
#8084 = AXIS2_PLACEMENT_3D ( 'NONE', #1911, #954, #12883 ) ;
#8083 = CARTESIAN_POINT ( 'NONE',  ( 178.0000000000000853, 15.03993994372673804, 38.07518420361041933 ) ) ;
#8085 = DIRECTION ( 'NONE',  ( 1.000000000000000000, 0.000000000000000000, 0.000000000000000000 ) ) ;
#8086 = CARTESIAN_POINT ( 'NONE',  ( -224.5839432122867834, 144.8618247958639245, 3.066209503615932697 ) ) ;
#8087 = ORIENTED_EDGE ( 'NONE', *, *, #2664, .T. ) ;
#8088 = ORIENTED_EDGE ( 'NONE', *, *, #13659, .T. ) ;
#8089 = CARTESIAN_POINT ( 'NONE',  ( 200.1062858801516597, 35.86394065090269123, 12.00000000000001066 ) ) ;
#8090 = DIRECTION ( 'NONE',  ( 0.000000000000000000, -1.000000000000000000, -1.486905836551548832E-16 ) ) ;
#8091 = EDGE_LOOP ( 'NONE', ( #664, #2459 ) ) ;
#8092 = CARTESIAN_POINT ( 'NONE',  ( -166.2149879755189659, 118.1214081567377150, 2.431557144026069928 ) ) ;
#8093 = AXIS2_PLACEMENT_3D ( 'NONE', #15540, #3801, #7215 ) ;
#8094 = VECTOR ( 'NONE', #7227, 1000.000000000000114 ) ;
#8095 = FACE_OUTER_BOUND ( 'NONE', #11461, .T. ) ;
#8096 = FACE_OUTER_BOUND ( 'NONE', #13480, .T. ) ;
#8097 = DIRECTION ( 'NONE',  ( 1.000000000000000000, 0.000000000000000000, 0.000000000000000000 ) ) ;
#8098 = EDGE_CURVE ( 'NONE', #13426, #7619, #12167, .T. ) ;
#8099 = EDGE_CURVE ( 'NONE', #12671, #14171, #14682, .T. ) ;
#8100 = ADVANCED_FACE ( 'NONE', ( #8862 ), #13650, .F. ) ;
#8101 = FACE_OUTER_BOUND ( 'NONE', #11339, .T. ) ;
#8102 = VECTOR ( 'NONE', #15373, 1000.000000000000114 ) ;
#8103 = ORIENTED_EDGE ( 'NONE', *, *, #13771, .T. ) ;
#8104 = CARTESIAN_POINT ( 'NONE',  ( 191.4922098844999425, 60.63967129342340456, 10.00000000000000178 ) ) ;
#8105 = CIRCLE ( 'NONE', #1019, 1.499999999999994449 ) ;
#8106 = CARTESIAN_POINT ( 'NONE',  ( -200.7948432279144129, 140.6912097071583787, -4.640918829492429509 ) ) ;
#8107 = CIRCLE ( 'NONE', #1266, 1.700000000000007061 ) ;
#8108 = DIRECTION ( 'NONE',  ( -3.965082230804130220E-16, 1.090924371466202084E-47, 1.000000000000000000 ) ) ;
#8109 = VERTEX_POINT ( 'NONE', #12543 ) ;
#8110 = CARTESIAN_POINT ( 'NONE',  ( -184.7739606708014719, 119.6463200498024548, -0.4555467707853387282 ) ) ;
#8111 = CARTESIAN_POINT ( 'NONE',  ( 201.5722569949026877, 29.04292258031605556, -3.626438834624695406 ) ) ;
#8112 = EDGE_LOOP ( 'NONE', ( #3808, #9971, #8088, #2951 ) ) ;
#8113 = CARTESIAN_POINT ( 'NONE',  ( -63.50000000000002842, 17.53993994372673271, 52.49999999999997868 ) ) ;
#8114 = CYLINDRICAL_SURFACE ( 'NONE', #5703, 8.000000000000028422 ) ;
#8115 = VECTOR ( 'NONE', #2044, 1000.000000000000000 ) ;
#8116 = CARTESIAN_POINT ( 'NONE',  ( -85.99999999999994316, 64.51493994372674479, 15.00000000000174794 ) ) ;
#8117 = CONICAL_SURFACE ( 'NONE', #1276, 8.000000000000028422, 1.047197551196600296 ) ;
#8118 = ORIENTED_EDGE ( 'NONE', *, *, #15476, .F. ) ;
#8119 = LINE ( 'NONE', #8033, #14908 ) ;
#8120 = ORIENTED_EDGE ( 'NONE', *, *, #8624, .F. ) ;
#8121 = LINE ( 'NONE', #11737, #4651 ) ;
#8122 = CARTESIAN_POINT ( 'NONE',  ( -173.3126422121597443, 122.7186289792270912, 10.06128868882609062 ) ) ;
#8123 = CARTESIAN_POINT ( 'NONE',  ( 5.196152422706632024, 9.000000000000003553, 5.000000000000000000 ) ) ;
#8124 = DIRECTION ( 'NONE',  ( 1.000000000000000000, -2.751328491981765035E-32, 3.965082230804130220E-16 ) ) ;
#8125 = EDGE_LOOP ( 'NONE', ( #5431, #11725, #15039, #4180, #12004, #8707, #14094, #5893 ) ) ;
#8127 = FACE_OUTER_BOUND ( 'NONE', #3799, .T. ) ;
#8126 = TOROIDAL_SURFACE ( 'NONE', #8385, 4.799128011492294732, 1.499999999999997113 ) ;
#8128 = ORIENTED_EDGE ( 'NONE', *, *, #2591, .T. ) ;
#8129 = ADVANCED_FACE ( 'NONE', ( #8940 ), #8704, .F. ) ;
#8130 = VERTEX_POINT ( 'NONE', #10196 ) ;
#8131 = CIRCLE ( 'NONE', #7105, 0.4999999999999996114 ) ;
#8132 = DIRECTION ( 'NONE',  ( 1.000000000000000000, 0.000000000000000000, 0.000000000000000000 ) ) ;
#8133 = LINE ( 'NONE', #7816, #5506 ) ;
#8134 = ADVANCED_FACE ( 'NONE', ( #2699, #12317, #1498 ), #13734, .T. ) ;
#8135 = FACE_OUTER_BOUND ( 'NONE', #5926, .T. ) ;
#8136 = CARTESIAN_POINT ( 'NONE',  ( -173.7035685021366476, 117.0154621025335899, 6.591438069051481996 ) ) ;
#8137 = CARTESIAN_POINT ( 'NONE',  ( -220.7684332601648407, 147.5206264611648805, -4.971276815939039473 ) ) ;
#8138 = LINE ( 'NONE', #13959, #9670 ) ;
#8139 = AXIS2_PLACEMENT_3D ( 'NONE', #10472, #13775, #15259 ) ;
#8140 = DIRECTION ( 'NONE',  ( 0.000000000000000000, 0.000000000000000000, 1.000000000000000000 ) ) ;
#8141 = CIRCLE ( 'NONE', #1303, 59.90987050789675550 ) ;
#8142 = DIRECTION ( 'NONE',  ( -1.000000000000000000, -2.751328491981765035E-32, 3.965082230804130220E-16 ) ) ;
#8143 = DIRECTION ( 'NONE',  ( -1.000000000000000000, 0.000000000000000000, 0.000000000000000000 ) ) ;
#8144 = DIRECTION ( 'NONE',  ( 0.000000000000000000, 0.000000000000000000, 1.000000000000000000 ) ) ;
#8145 = CARTESIAN_POINT ( 'NONE',  ( -85.99999999999994316, 59.53993994372674337, 15.00000000000174794 ) ) ;
#8146 = ORIENTED_EDGE ( 'NONE', *, *, #9692, .T. ) ;
#8147 = DIRECTION ( 'NONE',  ( 0.000000000000000000, 0.000000000000000000, 1.000000000000000000 ) ) ;
#8148 = EDGE_LOOP ( 'NONE', ( #12851, #13554, #2962, #5701 ) ) ;
#8149 = ADVANCED_FACE ( 'NONE', ( #1660 ), #14180, .F. ) ;
#8150 = CARTESIAN_POINT ( 'NONE',  ( 0.7145311798163258565, -9.237604307034018802, 2.775557561562891351E-14 ) ) ;
#8151 = DIRECTION ( 'NONE',  ( 0.000000000000000000, 0.000000000000000000, -1.000000000000000000 ) ) ;
#8152 = AXIS2_PLACEMENT_3D ( 'NONE', #6042, #3511, #8269 ) ;
#8153 = ORIENTED_EDGE ( 'NONE', *, *, #1829, .F. ) ;
#8154 = FILL_AREA_STYLE_COLOUR ( '', #6898 ) ;
#8155 = CARTESIAN_POINT ( 'NONE',  ( 164.0000000000000568, 59.53993994372674337, 13.29999999999999538 ) ) ;
#8156 = CIRCLE ( 'NONE', #13165, 3.299128011492291623 ) ;
#8158 = EDGE_LOOP ( 'NONE', ( #7762, #2625 ) ) ;
#8157 = EDGE_CURVE ( 'NONE', #10340, #427, #7138, .T. ) ;
#8159 = ORIENTED_EDGE ( 'NONE', *, *, #1505, .F. ) ;
#8160 = CARTESIAN_POINT ( 'NONE',  ( 188.3266922173125124, 39.20571348140700252, -7.512715813640810758 ) ) ;
#8161 = ADVANCED_FACE ( 'NONE', ( #13574 ), #2779, .F. ) ;
#8162 = DIRECTION ( 'NONE',  ( 0.000000000000000000, 0.000000000000000000, 1.000000000000000000 ) ) ;
#8163 = EDGE_LOOP ( 'NONE', ( #6743, #14267, #3897 ) ) ;
#8164 = VECTOR ( 'NONE', #220, 1000.000000000000000 ) ;
#8165 = CARTESIAN_POINT ( 'NONE',  ( 0.000000000000000000, 9.797174393178861156E-16, -8.000000000000028422 ) ) ;
#8166 = LINE ( 'NONE', #6969, #4553 ) ;
#8167 = CARTESIAN_POINT ( 'NONE',  ( -225.6729109059797338, 142.9107682335207983, 3.303491872377302574 ) ) ;
#8168 = ORIENTED_EDGE ( 'NONE', *, *, #8647, .T. ) ;
#8169 = ORIENTED_EDGE ( 'NONE', *, *, #2443, .F. ) ;
#8170 = DIRECTION ( 'NONE',  ( 0.000000000000000000, 0.000000000000000000, 1.000000000000000000 ) ) ;
#8171 = DIRECTION ( 'NONE',  ( 0.000000000000000000, 0.000000000000000000, 1.000000000000000000 ) ) ;
#8172 = CIRCLE ( 'NONE', #12172, 3.525000000000000355 ) ;
#8173 = EDGE_CURVE ( 'NONE', #11071, #1328, #2851, .T. ) ;
#8174 = ORIENTED_EDGE ( 'NONE', *, *, #7515, .T. ) ;
#8175 = DIRECTION ( 'NONE',  ( 0.8660254037844388186, -0.4999999999999997780, 0.000000000000000000 ) ) ;
#8176 = FACE_OUTER_BOUND ( 'NONE', #4857, .T. ) ;
#8177 = CIRCLE ( 'NONE', #13947, 1.700000000000007061 ) ;
#8178 = FACE_OUTER_BOUND ( 'NONE', #8582, .T. ) ;
#8179 = EDGE_LOOP ( 'NONE', ( #2636, #6766, #6937, #6669 ) ) ;
#8180 = ADVANCED_FACE ( 'NONE', ( #4253, #12702 ), #11531, .F. ) ;
#8181 = DIRECTION ( 'NONE',  ( 1.000000000000000000, 2.751328491981765035E-32, -3.965082230804130220E-16 ) ) ;
#8182 = CARTESIAN_POINT ( 'NONE',  ( -169.9318100387881714, 128.7846982781319412, 2.500000000781056997 ) ) ;
#8183 = DIRECTION ( 'NONE',  ( -0.000000000000000000, 1.000000000000000000, 1.156482317317871725E-16 ) ) ;
#8184 = EDGE_LOOP ( 'NONE', ( #12436, #1805, #14450, #4367 ) ) ;
#8185 = CARTESIAN_POINT ( 'NONE',  ( -211.5558396979514839, 139.0314540006070274, -4.642206099735020963 ) ) ;
#8186 = UNCERTAINTY_MEASURE_WITH_UNIT (LENGTH_MEASURE( 1.000000000000000082E-05 ), #3150, 'distance_accuracy_value', 'NONE');
#8187 = CARTESIAN_POINT ( 'NONE',  ( 205.3852585099181454, 47.89158942159311039, -8.629264428576009394 ) ) ;
#8188 = AXIS2_PLACEMENT_3D ( 'NONE', #14972, #10334, #6559 ) ;
#8189 = ORIENTED_EDGE ( 'NONE', *, *, #4874, .T. ) ;
#8191 = ADVANCED_FACE ( 'NONE', ( #693 ), #56, .T. ) ;
#8190 = EDGE_CURVE ( 'NONE', #12405, #176, #7404, .T. ) ;
#8192 = ADVANCED_FACE ( 'NONE', ( #3090 ), #3161, .F. ) ;
#8193 = DIRECTION ( 'NONE',  ( -1.000000000000000000, 0.000000000000000000, 3.965082230804112963E-16 ) ) ;
#8194 = CARTESIAN_POINT ( 'NONE',  ( 7.375539388216818230E-16, -0.2686526913914984438, -2.750000000000000888 ) ) ;
#8195 = ADVANCED_FACE ( 'NONE', ( #6728 ), #9095, .F. ) ;
#8196 = CARTESIAN_POINT ( 'NONE',  ( -150.4353350883832832, 107.0093798342911242, -4.794633519332702321 ) ) ;
#8197 = VERTEX_POINT ( 'NONE', #10349 ) ;
#8198 = CIRCLE ( 'NONE', #7683, 0.5000000000000004441 ) ;
#8199 = CARTESIAN_POINT ( 'NONE',  ( 190.5000000000000853, 16.03993994372673981, 24.94742576086838781 ) ) ;
#8200 = CARTESIAN_POINT ( 'NONE',  ( 191.4322133549729585, 42.19665789901188901, -4.493471110936619439 ) ) ;
#8201 = VERTEX_POINT ( 'NONE', #9325 ) ;
#8202 = CARTESIAN_POINT ( 'NONE',  ( -35.99999999999995026, 64.53993994372673626, 15.00000000000139977 ) ) ;
#8203 = TOROIDAL_SURFACE ( 'NONE', #12456, 1.000000000000000000, 0.5000000000000000000 ) ;
#8204 = CARTESIAN_POINT ( 'NONE',  ( -205.9652191273047777, 131.2378527988410326, 3.478895870929496148 ) ) ;
#8205 = CARTESIAN_POINT ( 'NONE',  ( -130.9946291778373961, 96.97121815129470690, 0.000000000000000000 ) ) ;
#8206 = CARTESIAN_POINT ( 'NONE',  ( 15.71029453487719074, 40.04259805664093363, 5.000000000000000000 ) ) ;
#8207 = CARTESIAN_POINT ( 'NONE',  ( 5.799999999999999822, 7.999999999999979572, 0.000000000000000000 ) ) ;
#8208 = EDGE_CURVE ( 'NONE', #1269, #4524, #6398, .T. ) ;
#8209 = ORIENTED_EDGE ( 'NONE', *, *, #3824, .F. ) ;
#8210 = ORIENTED_EDGE ( 'NONE', *, *, #12398, .T. ) ;
#8211 = CARTESIAN_POINT ( 'NONE',  ( 184.0000000000000568, 15.53993994372673626, 47.49999999999997868 ) ) ;
#8212 = CARTESIAN_POINT ( 'NONE',  ( 178.0000000000000853, 15.53993994372673626, 52.49999999999997868 ) ) ;
#8213 = AXIS2_PLACEMENT_3D ( 'NONE', #2012, #5732, #1855 ) ;
#8214 = PLANE ( 'NONE',  #6402 ) ;
#8215 = CARTESIAN_POINT ( 'NONE',  ( 114.0000000000000568, 64.53993994372673626, 18.52500000000035385 ) ) ;
#8216 = CARTESIAN_POINT ( 'NONE',  ( -222.7110019469168662, 143.7735985160120151, -2.692100231736752391 ) ) ;
#8217 = CARTESIAN_POINT ( 'NONE',  ( -217.0204816151944840, 154.3338338561956391, 5.540248425174711500 ) ) ;
#8218 = CARTESIAN_POINT ( 'NONE',  ( -216.6980668629938123, 154.8869363267023687, 2.500000000158653091 ) ) ;
#8219 = CARTESIAN_POINT ( 'NONE',  ( 171.7208925888976978, 62.57671370024034729, -0.9107274384406883749 ) ) ;
#8220 = DIRECTION ( 'NONE',  ( 1.000000000000000000, 0.000000000000000000, 0.000000000000000000 ) ) ;
#8221 = EDGE_CURVE ( 'NONE', #6887, #101, #11612, .T. ) ;
#8222 = CIRCLE ( 'NONE', #9729, 1.699999999999993072 ) ;
#8223 = DIRECTION ( 'NONE',  ( 1.000000000000000000, 0.000000000000000000, 3.965082230804112963E-16 ) ) ;
#8224 = CARTESIAN_POINT ( 'NONE',  ( -64.00000000000002842, -178.8058001507315566, -17.19066787724516843 ) ) ;
#8225 = DIRECTION ( 'NONE',  ( 0.000000000000000000, 0.000000000000000000, 1.000000000000000000 ) ) ;
#8226 = EDGE_LOOP ( 'NONE', ( #7383, #4309, #4608, #8945, #154 ) ) ;
#8227 = ORIENTED_EDGE ( 'NONE', *, *, #15166, .T. ) ;
#8228 = DIRECTION ( 'NONE',  ( -0.000000000000000000, -0.000000000000000000, -1.000000000000000000 ) ) ;
#8229 = CARTESIAN_POINT ( 'NONE',  ( -216.7216729069047005, 154.8463875879168086, 3.280095325655492111 ) ) ;
#8230 = ORIENTED_EDGE ( 'NONE', *, *, #5337, .F. ) ;
#8231 = DIRECTION ( 'NONE',  ( -1.000000000000000000, -2.751328491981765035E-32, 3.965082230804130220E-16 ) ) ;
#8232 = LINE ( 'NONE', #13009, #11870 ) ;
#8233 = AXIS2_PLACEMENT_3D ( 'NONE', #1275, #82, #15072 ) ;
#8234 = VERTEX_POINT ( 'NONE', #777 ) ;
#8235 = ORIENTED_EDGE ( 'NONE', *, *, #13462, .F. ) ;
#8236 = EDGE_CURVE ( 'NONE', #12968, #7962, #1583, .T. ) ;
#8237 = CYLINDRICAL_SURFACE ( 'NONE', #14407, 0.5000000000000001110 ) ;
#8238 = B_SPLINE_CURVE_WITH_KNOTS ( 'NONE', 3,
 ( #11430, #13544, #8752, #9943, #594, #5432, #4230, #9069, #14734, #3930, #12372, #1557, #12834, #909, #11512, #5739, #13950, #9223 ),
 .UNSPECIFIED., .F., .F.,
 ( 4, 2, 2, 2, 2, 2, 2, 2, 4 ),
 ( 0.003229178684347154982, 0.003627155556181206521, 0.004025132428015258494, 0.004423109299849310033, 0.004821086171683361572, 0.005219063043517413111, 0.005617039915351465518, 0.006015016787185517057, 0.006412993659019568596 ),
 .UNSPECIFIED. ) ;
#8239 = ORIENTED_EDGE ( 'NONE', *, *, #2924, .F. ) ;
#8240 = DIRECTION ( 'NONE',  ( 0.000000000000000000, 0.7071067811864985009, 0.7071067811865965336 ) ) ;
#8241 = FACE_OUTER_BOUND ( 'NONE', #11230, .T. ) ;
#8242 = EDGE_LOOP ( 'NONE', ( #7361, #8598, #487, #8153 ) ) ;
#8243 = ORIENTED_EDGE ( 'NONE', *, *, #10623, .T. ) ;
#8244 = LINE ( 'NONE', #4507, #13819 ) ;
#8245 = DIRECTION ( 'NONE',  ( -3.965082230804130220E-16, 4.956352788505162775E-17, -1.000000000000000000 ) ) ;
#8246 = VERTEX_POINT ( 'NONE', #8072 ) ;
#8247 = DIRECTION ( 'NONE',  ( -0.000000000000000000, -0.000000000000000000, 1.000000000000000000 ) ) ;
#8248 = CARTESIAN_POINT ( 'NONE',  ( 171.7208925888976978, 62.57671370024034729, -0.9107274384406883749 ) ) ;
#8249 = AXIS2_PLACEMENT_3D ( 'NONE', #12993, #10960, #3527 ) ;
#8250 = VERTEX_POINT ( 'NONE', #15063 ) ;
#8251 = ADVANCED_FACE ( 'NONE', ( #2046 ), #11693, .T. ) ;
#8252 = DIRECTION ( 'NONE',  ( 0.000000000000000000, -1.486905836551548832E-16, 1.000000000000000000 ) ) ;
#8253 = EDGE_CURVE ( 'NONE', #14543, #13828, #857, .T. ) ;
#8254 = ORIENTED_EDGE ( 'NONE', *, *, #14587, .F. ) ;
#8255 = DIRECTION ( 'NONE',  ( 0.000000000000000000, 4.956352788505162775E-17, -1.000000000000000000 ) ) ;
#8256 = CARTESIAN_POINT ( 'NONE',  ( -187.9132138465967898, 138.8208849330412988, 2.500000000000000000 ) ) ;
#8257 = DIRECTION ( 'NONE',  ( 0.000000000000000000, 0.000000000000000000, 1.000000000000000000 ) ) ;
#8258 = ORIENTED_EDGE ( 'NONE', *, *, #364, .T. ) ;
#8259 = CARTESIAN_POINT ( 'NONE',  ( -185.2102393155530535, 125.0770951282925409, -4.642206099734998759 ) ) ;
#8260 = CARTESIAN_POINT ( 'NONE',  ( 207.1750190499664370, 35.67744599754978907, -6.373597270514506974 ) ) ;
#8261 = EDGE_LOOP ( 'NONE', ( #15148, #5447, #1424, #6563 ) ) ;
#8262 = DIRECTION ( 'NONE',  ( 0.000000000000000000, 1.000000000000000000, -0.000000000000000000 ) ) ;
#8263 = DIRECTION ( 'NONE',  ( 0.000000000000000000, -0.1391731009600592484, 0.9902680687415712502 ) ) ;
#8264 = EDGE_CURVE ( 'NONE', #5867, #5228, #9669, .T. ) ;
#8265 = CARTESIAN_POINT ( 'NONE',  ( -76.00000000000001421, 15.53993994372673981, -3.075184203610571654 ) ) ;
#8266 = ORIENTED_EDGE ( 'NONE', *, *, #7158, .T. ) ;
#8267 =( NAMED_UNIT ( * ) PLANE_ANGLE_UNIT ( ) SI_UNIT ( $, .RADIAN. ) );
#8268 = EDGE_CURVE ( 'NONE', #1469, #6998, #2752, .T. ) ;
#8269 = DIRECTION ( 'NONE',  ( -1.000000000000000000, 0.000000000000000000, 0.000000000000000000 ) ) ;
#8270 = CARTESIAN_POINT ( 'NONE',  ( 193.1249951165660548, 46.22013307728793308, -3.310989833511668756 ) ) ;
#8271 = ORIENTED_EDGE ( 'NONE', *, *, #4974, .T. ) ;
#8272 = CYLINDRICAL_SURFACE ( 'NONE', #13720, 325.5619230110239073 ) ;
#8273 = CARTESIAN_POINT ( 'NONE',  ( -176.6594047394515314, 116.7136007993067324, 1.317773660835219740 ) ) ;
#8274 = ADVANCED_FACE ( 'NONE', ( #353 ), #2833, .F. ) ;
#8275 = CARTESIAN_POINT ( 'NONE',  ( -76.50000000000001421, 15.47035339324671099, -2.004865965629286872 ) ) ;
#8276 = EDGE_CURVE ( 'NONE', #701, #10197, #11182, .T. ) ;
#8277 = DIRECTION ( 'NONE',  ( 0.5602235199536453880, 0.8138631617988981715, 0.1541958545404129299 ) ) ;
#8278 = CARTESIAN_POINT ( 'NONE',  ( 208.8186272397570349, 39.68461847005694665, -7.558035125831273682 ) ) ;
#8279 = EDGE_LOOP ( 'NONE', ( #6215, #5410, #14643, #1635 ) ) ;
#8280 = EDGE_LOOP ( 'NONE', ( #11760, #6686, #11839, #4719 ) ) ;
#8281 = CARTESIAN_POINT ( 'NONE',  ( 202.8882743124338504, 32.81631024066724933, -8.087096619718394663 ) ) ;
#8282 = DIRECTION ( 'NONE',  ( -0.000000000000000000, -0.000000000000000000, 1.000000000000000000 ) ) ;
#8283 = CARTESIAN_POINT ( 'NONE',  ( -64.00000000000002842, 15.03993994372673804, 24.94742576086838781 ) ) ;
#8284 = CARTESIAN_POINT ( 'NONE',  ( -63.50000000000002842, -181.3058001507315566, 84.88378295107885663 ) ) ;
#8285 = CARTESIAN_POINT ( 'NONE',  ( -224.1052059540971584, 145.7195577429836817, -0.7975646621416776494 ) ) ;
#8286 = AXIS2_PLACEMENT_3D ( 'NONE', #2033, #3307, #6946 ) ;
#8287 = CARTESIAN_POINT ( 'NONE',  ( -222.8281890163352159, 143.5973427195760905, 7.369092821369231494 ) ) ;
#8288 = EDGE_CURVE ( 'NONE', #4350, #13543, #7492, .T. ) ;
#8289 = ADVANCED_FACE ( 'NONE', ( #7815 ), #8660, .F. ) ;
#8290 = EDGE_CURVE ( 'NONE', #3756, #2220, #4154, .T. ) ;
#8291 = DIRECTION ( 'NONE',  ( 1.000000000000000000, 0.000000000000000000, 0.000000000000000000 ) ) ;
#8292 = DIRECTION ( 'NONE',  ( 3.965082230804130220E-16, 1.090924371466202084E-47, 1.000000000000000000 ) ) ;
#8293 = CARTESIAN_POINT ( 'NONE',  ( -76.00000000000001421, 16.03993994372673981, -7.458121719691109004E-14 ) ) ;
#8294 = AXIS2_PLACEMENT_3D ( 'NONE', #4431, #14059, #2143 ) ;
#8295 = DIRECTION ( 'NONE',  ( 0.000000000000000000, 0.9902680687415714722, -0.1391731009600582769 ) ) ;
#8296 = LINE ( 'NONE', #11834, #11400 ) ;
#8297 = ORIENTED_EDGE ( 'NONE', *, *, #4994, .F. ) ;
#8298 = AXIS2_PLACEMENT_3D ( 'NONE', #47, #4884, #9703 ) ;
#8299 = VERTEX_POINT ( 'NONE', #8994 ) ;
#8300 = FACE_OUTER_BOUND ( 'NONE', #14886, .T. ) ;
#8301 = CARTESIAN_POINT ( 'NONE',  ( 64.00000000000005684, 64.51493994372674479, 11.50000000000069811 ) ) ;
#8302 = CARTESIAN_POINT ( 'NONE',  ( -76.50000000000001421, 15.53993994372673981, -17.50000000000002487 ) ) ;
#8303 = DIRECTION ( 'NONE',  ( -0.000000000000000000, 0.000000000000000000, 1.000000000000000000 ) ) ;
#8304 = PRODUCT_DEFINITION_SHAPE ( 'NONE', 'NONE',  #15631 ) ;
#8305 = EDGE_CURVE ( 'NONE', #2220, #7302, #12521, .T. ) ;
#8306 = VECTOR ( 'NONE', #1401, 1000.000000000000114 ) ;
#8307 = PRODUCT_DEFINITION_FORMATION_WITH_SPECIFIED_SOURCE ( 'ANY', '', #9174, .NOT_KNOWN. ) ;
#8308 = ORIENTED_EDGE ( 'NONE', *, *, #11695, .T. ) ;
#8309 = CIRCLE ( 'NONE', #3495, 1.700000000000007061 ) ;
#8310 = VERTEX_POINT ( 'NONE', #14803 ) ;
#8311 = CARTESIAN_POINT ( 'NONE',  ( 202.8426534586648700, 48.90729187601812811, -2.475854291071949209 ) ) ;
#8312 = SURFACE_STYLE_USAGE ( .BOTH. , #7280 ) ;
#8313 = ORIENTED_EDGE ( 'NONE', *, *, #15238, .F. ) ;
#8314 = CARTESIAN_POINT ( 'NONE',  ( -225.2374285875299620, 143.6910031662873735, 6.106889910990925152 ) ) ;
#8315 = ORIENTED_EDGE ( 'NONE', *, *, #7503, .F. ) ;
#8316 = TOROIDAL_SURFACE ( 'NONE', #7518, 1.000000000000000000, 0.5000000000000000000 ) ;
#8317 = ORIENTED_EDGE ( 'NONE', *, *, #3303, .F. ) ;
#8318 = CYLINDRICAL_SURFACE ( 'NONE', #10319, 1.499999999999997780 ) ;
#8319 = DIRECTION ( 'NONE',  ( 0.000000000000000000, 0.000000000000000000, -1.000000000000000000 ) ) ;
#8320 = VECTOR ( 'NONE', #11159, 1000.000000000000000 ) ;
#8321 = EDGE_LOOP ( 'NONE', ( #3399, #15108, #3334, #1045 ) ) ;
#8322 = DIRECTION ( 'NONE',  ( 0.000000000000000000, 1.000000000000000000, 0.000000000000000000 ) ) ;
#8323 = ADVANCED_FACE ( 'NONE', ( #10247 ), #8832, .F. ) ;
#8324 = CARTESIAN_POINT ( 'NONE',  ( -164.5262273476079713, 106.7842295329138835, 0.000000000000000000 ) ) ;
#8325 = AXIS2_PLACEMENT_3D ( 'NONE', #968, #6994, #6840 ) ;
#8326 = VERTEX_POINT ( 'NONE', #13628 ) ;
#8327 = SURFACE_STYLE_FILL_AREA ( #15317 ) ;
#8328 = VERTEX_POINT ( 'NONE', #11275 ) ;
#8329 = DIRECTION ( 'NONE',  ( -0.000000000000000000, -0.000000000000000000, 1.000000000000000000 ) ) ;
#8330 = CARTESIAN_POINT ( 'NONE',  ( 114.0000000000000568, 64.53993994372673626, 13.30000000000035776 ) ) ;
#8331 = EDGE_CURVE ( 'NONE', #5911, #9609, #10021, .T. ) ;
#8332 = DIRECTION ( 'NONE',  ( 0.000000000000000000, 0.000000000000000000, -1.000000000000000000 ) ) ;
#8333 = AXIS2_PLACEMENT_3D ( 'NONE', #7010, #14483, #7093 ) ;
#8334 = EDGE_LOOP ( 'NONE', ( #11564, #1972, #14575, #1431 ) ) ;
#8335 = CARTESIAN_POINT ( 'NONE',  ( -176.9844935205031504, 127.5518652045528825, -4.662307221713766658 ) ) ;
#8336 = CARTESIAN_POINT ( 'NONE',  ( 207.0671064858421744, 46.21029813590134694, -8.754270687730807410 ) ) ;
#8337 = COLOUR_RGB ( '', 0.08235294, 0.09019608, 0.10196078) ;
#8338 = EDGE_LOOP ( 'NONE', ( #1463, #14858, #1171, #11402 ) ) ;
#8339 = AXIS2_PLACEMENT_3D ( 'NONE', #5046, #14581, #9786 ) ;
#8340 = AXIS2_PLACEMENT_3D ( 'NONE', #716, #11786, #641 ) ;
#8341 = FACE_BOUND ( 'NONE', #7477, .T. ) ;
#8342 = DIRECTION ( 'NONE',  ( 0.000000000000000000, 0.000000000000000000, -1.000000000000000000 ) ) ;
#8343 = CARTESIAN_POINT ( 'NONE',  ( 190.5000000000000568, -179.8058001507315566, -51.45141194869120227 ) ) ;
#8344 = VECTOR ( 'NONE', #15312, 1000.000000000000000 ) ;
#8345 = VERTEX_POINT ( 'NONE', #6550 ) ;
#8346 = EDGE_CURVE ( 'NONE', #13140, #5990, #12448, .T. ) ;
#8347 = CIRCLE ( 'NONE', #1518, 0.5000000000000004441 ) ;
#8348 = PRODUCT_CONTEXT ( 'NONE', #7496, 'mechanical' ) ;
#8349 = CARTESIAN_POINT ( 'NONE',  ( 207.1131222881253393, 35.56952893079440514, -7.807171136772324438 ) ) ;
#8350 = VERTEX_POINT ( 'NONE', #6308 ) ;
#8351 = DIRECTION ( 'NONE',  ( 0.000000000000000000, 0.1391731009600592484, 0.9902680687415712502 ) ) ;
#8352 = LINE ( 'NONE', #6047, #618 ) ;
#8353 = CARTESIAN_POINT ( 'NONE',  ( -187.5349220100912930, 120.9938564418671518, 3.478895870929501921 ) ) ;
#8354 = DIRECTION ( 'NONE',  ( 1.000000000000000000, 0.000000000000000000, 0.000000000000000000 ) ) ;
#8355 = DIRECTION ( 'NONE',  ( -0.9741547192086869034, 0.2258817899775114879, 0.000000000000000000 ) ) ;
#8356 = FACE_BOUND ( 'NONE', #3816, .T. ) ;
#8357 = ORIENTED_EDGE ( 'NONE', *, *, #1026, .T. ) ;
#8358 = ORIENTED_EDGE ( 'NONE', *, *, #11075, .F. ) ;
#8359 = VECTOR ( 'NONE', #12856, 1000.000000000000000 ) ;
#8360 = FACE_OUTER_BOUND ( 'NONE', #3957, .T. ) ;
#8361 = CARTESIAN_POINT ( 'NONE',  ( 190.5000000000000568, 19.53993994372674337, 9.999999999999998224 ) ) ;
#8362 = AXIS2_PLACEMENT_3D ( 'NONE', #14016, #7963, #12914 ) ;
#8363 = EDGE_CURVE ( 'NONE', #7029, #3604, #14568, .T. ) ;
#8364 = DIRECTION ( 'NONE',  ( 0.000000000000000000, -0.1391731009600592484, 0.9902680687415712502 ) ) ;
#8365 = DIRECTION ( 'NONE',  ( -0.000000000000000000, 1.000000000000000000, 0.000000000000000000 ) ) ;
#8366 = CARTESIAN_POINT ( 'NONE',  ( -221.4260126471363037, 146.2653786650752181, -4.596864862611049318 ) ) ;
#8367 = CARTESIAN_POINT ( 'NONE',  ( -220.2684726731945943, 148.5160382146572999, 9.961107950553353518 ) ) ;
#8368 = DIRECTION ( 'NONE',  ( 0.000000000000000000, 1.224646799147353207E-16, 1.000000000000000000 ) ) ;
#8369 = CIRCLE ( 'NONE', #5826, 2.749999999999999112 ) ;
#8370 = DIRECTION ( 'NONE',  ( 1.000000000000000000, -2.751328491981765035E-32, 3.965082230804130220E-16 ) ) ;
#8371 = LINE ( 'NONE', #2506, #15615 ) ;
#8372 = CARTESIAN_POINT ( 'NONE',  ( 184.0000000000000568, 17.53993994372673981, -10.99999999999999822 ) ) ;
#8373 = CIRCLE ( 'NONE', #3066, 1.500000000000001332 ) ;
#8374 = CARTESIAN_POINT ( 'NONE',  ( 5.000000000000000000, 6.123233995736766282E-16, 5.000000000000000000 ) ) ;
#8375 = ORIENTED_EDGE ( 'NONE', *, *, #9637, .T. ) ;
#8376 = ORIENTED_EDGE ( 'NONE', *, *, #4567, .T. ) ;
#8377 = DIRECTION ( 'NONE',  ( -0.000000000000000000, -0.9902680687415705840, -0.1391731009600641333 ) ) ;
#8378 = DIRECTION ( 'NONE',  ( 0.000000000000000000, 0.9902680687415710281, -0.1391731009600611635 ) ) ;
#8379 = DIRECTION ( 'NONE',  ( -1.000000000000000000, 0.000000000000000000, 0.000000000000000000 ) ) ;
#8380 = EDGE_CURVE ( 'NONE', #8424, #4152, #12601, .T. ) ;
#8381 = DIRECTION ( 'NONE',  ( 1.000000000000000000, 2.751328491981765035E-32, -3.965082230804130220E-16 ) ) ;
#8382 = DIRECTION ( 'NONE',  ( -0.000000000000000000, -0.000000000000000000, -1.000000000000000000 ) ) ;
#8384 = EDGE_CURVE ( 'NONE', #14712, #1333, #8238, .T. ) ;
#8383 = ADVANCED_FACE ( 'NONE', ( #11126 ), #10172, .T. ) ;
#8385 = AXIS2_PLACEMENT_3D ( 'NONE', #4809, #2041, #14270 ) ;
#8386 = CARTESIAN_POINT ( 'NONE',  ( -157.6477983077465694, 110.1970436846185066, 5.000000000000004441 ) ) ;
#8387 = CARTESIAN_POINT ( 'NONE',  ( -206.0179204244930702, 148.9258921110169638, 2.500000000000000000 ) ) ;
#8388 = APPLICATION_CONTEXT ( 'automotive_design' ) ;
#8389 = CIRCLE ( 'NONE', #12902, 1.699999999999993072 ) ;
#8390 = ORIENTED_EDGE ( 'NONE', *, *, #5973, .T. ) ;
#8391 = CONTEXT_DEPENDENT_SHAPE_REPRESENTATION ( #7879, #11423 ) ;
#8392 = VERTEX_POINT ( 'NONE', #2022 ) ;
#8393 = CARTESIAN_POINT ( 'NONE',  ( 203.1427736312160164, 48.80054947466439330, -2.493724563924679671 ) ) ;
#8394 = CARTESIAN_POINT ( 'NONE',  ( -61.94838851346079167, -178.8058001507315566, 52.19066787724494816 ) ) ;
#8395 = VERTEX_POINT ( 'NONE', #5666 ) ;
#8396 = FACE_BOUND ( 'NONE', #15020, .T. ) ;
#8397 = VECTOR ( 'NONE', #3125, 1000.000000000000000 ) ;
#8398 = CARTESIAN_POINT ( 'NONE',  ( -222.4225350102570928, 144.3966517966595973, 8.264308561663218811 ) ) ;
#8399 = ORIENTED_EDGE ( 'NONE', *, *, #5673, .T. ) ;
#8400 = ORIENTED_EDGE ( 'NONE', *, *, #14212, .F. ) ;
#8401 = AXIS2_PLACEMENT_3D ( 'NONE', #6225, #2669, #14655 ) ;
#8402 = PLANE ( 'NONE',  #14825 ) ;
#8403 = DIRECTION ( 'NONE',  ( 0.000000000000000000, 0.000000000000000000, 1.000000000000000000 ) ) ;
#8404 = ORIENTED_EDGE ( 'NONE', *, *, #10975, .F. ) ;
#8405 = DIRECTION ( 'NONE',  ( 0.000000000000000000, 0.000000000000000000, -1.000000000000000000 ) ) ;
#8406 = PLANE ( 'NONE',  #14430 ) ;
#8408 = CIRCLE ( 'NONE', #2340, 1.499999999999994449 ) ;
#8407 = VECTOR ( 'NONE', #2070, 1000.000000000000000 ) ;
#8409 = ORIENTED_EDGE ( 'NONE', *, *, #10450, .T. ) ;
#8410 = VERTEX_POINT ( 'NONE', #7894 ) ;
#8411 = CYLINDRICAL_SURFACE ( 'NONE', #15242, 4.499999999999950262 ) ;
#8412 = EDGE_CURVE ( 'NONE', #176, #12405, #1221, .T. ) ;
#8413 = LINE ( 'NONE', #9504, #12861 ) ;
#8414 = CARTESIAN_POINT ( 'NONE',  ( -70.00000000000000000, 17.53993994372673626, 45.99999999999998579 ) ) ;
#8415 = ORIENTED_EDGE ( 'NONE', *, *, #9015, .F. ) ;
#8416 = ORIENTED_EDGE ( 'NONE', *, *, #7764, .F. ) ;
#8417 = CARTESIAN_POINT ( 'NONE',  ( -215.7895908902557380, 152.2252679817794956, -2.963320117457100444 ) ) ;
#8418 = CARTESIAN_POINT ( 'NONE',  ( 208.8119396302737130, 39.73295740579614943, -6.128637076002331874 ) ) ;
#8419 = ORIENTED_EDGE ( 'NONE', *, *, #3261, .T. ) ;
#8420 = DIRECTION ( 'NONE',  ( 0.000000000000000000, 0.000000000000000000, -1.000000000000000000 ) ) ;
#8421 = CARTESIAN_POINT ( 'NONE',  ( -171.0277344788851792, 115.6541280562350806, 2.431557144026069928 ) ) ;
#8422 = CARTESIAN_POINT ( 'NONE',  ( 152.8671246545933400, 7.480744990243093362, -7.157132912367466737 ) ) ;
#8423 = AXIS2_PLACEMENT_3D ( 'NONE', #11824, #14256, #2263 ) ;
#8424 = VERTEX_POINT ( 'NONE', #4391 ) ;
#8425 = APPLICATION_PROTOCOL_DEFINITION ( 'draft international standard', 'automotive_design', 1998, #9917 ) ;
#8426 = FILL_AREA_STYLE ('',( #15495 ) ) ;
#8427 = EDGE_CURVE ( 'NONE', #7532, #9928, #3990, .T. ) ;
#8428 = CARTESIAN_POINT ( 'NONE',  ( 205.4496313998743915, 47.84832575209421890, -7.060263518810960370 ) ) ;
#8429 = ORIENTED_EDGE ( 'NONE', *, *, #10376, .T. ) ;
#8430 = CARTESIAN_POINT ( 'NONE',  ( -144.0627431139473345, 95.36268816863731956, 5.000000000000000000 ) ) ;
#8431 = DIRECTION ( 'NONE',  ( 0.000000000000000000, 1.000000000000000000, 0.000000000000000000 ) ) ;
#8432 = VECTOR ( 'NONE', #3940, 1000.000000000000000 ) ;
#8433 = CARTESIAN_POINT ( 'NONE',  ( -213.7863261933728154, 135.0464837791089963, 5.434137442415932995 ) ) ;
#8434 = CARTESIAN_POINT ( 'NONE',  ( 190.5000000000000853, 19.53993994372673626, 52.49999999999997868 ) ) ;
#8435 = ORIENTED_EDGE ( 'NONE', *, *, #4535, .F. ) ;
#8436 = CARTESIAN_POINT ( 'NONE',  ( -195.8085210632896178, 134.3768662836672547, 10.16010209732750269 ) ) ;
#8437 = CARTESIAN_POINT ( 'NONE',  ( 191.4249991583111523, 42.11970308376083949, -6.062475933048471433 ) ) ;
#8438 = EDGE_LOOP ( 'NONE', ( #7653, #8399, #11485 ) ) ;
#8439 = ORIENTED_EDGE ( 'NONE', *, *, #889, .T. ) ;
#8440 = CARTESIAN_POINT ( 'NONE',  ( -176.8865658880463343, 116.7841877362952943, 2.239335837349317071 ) ) ;
#8441 = DIRECTION ( 'NONE',  ( -0.000000000000000000, 1.000000000000000000, -0.000000000000000000 ) ) ;
#8442 = DIRECTION ( 'NONE',  ( 0.000000000000000000, 0.000000000000000000, 1.000000000000000000 ) ) ;
#8443 = FACE_OUTER_BOUND ( 'NONE', #888, .T. ) ;
#8444 = CARTESIAN_POINT ( 'NONE',  ( -223.4286909205997063, 142.3693733871445488, -0.01250108018631108930 ) ) ;
#8445 = CIRCLE ( 'NONE', #7182, 8.000000000000028422 ) ;
#8446 = CARTESIAN_POINT ( 'NONE',  ( -221.6474553585480578, 145.9023062856681179, 9.325220120579155392 ) ) ;
#8447 = CARTESIAN_POINT ( 'NONE',  ( -110.0000000000000426, 59.53993994372674337, 25.00000000000000000 ) ) ;
#8448 = CARTESIAN_POINT ( 'NONE',  ( -155.8458404752088313, 109.5861341462257172, 9.538603418629666209 ) ) ;
#8449 = EDGE_CURVE ( 'NONE', #15218, #12185, #6023, .T. ) ;
#8450 = CARTESIAN_POINT ( 'NONE',  ( -157.0972765366304316, 120.0943610593438251, 5.000000000000000000 ) ) ;
#8451 = DIRECTION ( 'NONE',  ( -0.000000000000000000, 1.000000000000000000, 1.156482317317871725E-16 ) ) ;
#8452 = DIRECTION ( 'NONE',  ( 1.000000000000000000, 0.000000000000000000, 0.000000000000000000 ) ) ;
#8453 = VERTEX_POINT ( 'NONE', #10327 ) ;
#8454 = AXIS2_PLACEMENT_3D ( 'NONE', #14031, #15280, #12998 ) ;
#8455 = EDGE_LOOP ( 'NONE', ( #4280, #13616, #3557, #2308 ) ) ;
#8456 = CARTESIAN_POINT ( 'NONE',  ( 17.41029453487719181, 40.04259805664093363, 0.000000000000000000 ) ) ;
#8457 = CARTESIAN_POINT ( 'NONE',  ( 190.5000000000000853, -179.3753867012116530, 64.38864891670806401 ) ) ;
#8458 = CARTESIAN_POINT ( 'NONE',  ( 190.5000000000000568, 16.03993994372673981, -17.50000000000002487 ) ) ;
#8459 = DIRECTION ( 'NONE',  ( -0.000000000000000000, 1.000000000000000000, 1.156482317317871725E-16 ) ) ;
#8460 = CARTESIAN_POINT ( 'NONE',  ( -83.77455057502459113, 65.19100426474074084, -20.00000000000000000 ) ) ;
#8461 = CARTESIAN_POINT ( 'NONE',  ( -172.3582205330567945, 130.1389812296867774, 2.500000000525777644 ) ) ;
#8463 = ORIENTED_EDGE ( 'NONE', *, *, #253, .F. ) ;
#8462 = EDGE_CURVE ( 'NONE', #1700, #1434, #842, .T. ) ;
#8464 = EDGE_LOOP ( 'NONE', ( #12971, #13433, #3574, #6175 ) ) ;
#8465 = CARTESIAN_POINT ( 'NONE',  ( 193.0579178353149246, 46.09544038230585272, -7.876361695281355324 ) ) ;
#8466 = PRODUCT_RELATED_PRODUCT_CATEGORY ( 'part', '', ( #15450 ) ) ;
#8467 = CARTESIAN_POINT ( 'NONE',  ( 190.0000000000000568, 15.03993994372673981, -3.075184203610571654 ) ) ;
#8468 = ORIENTED_EDGE ( 'NONE', *, *, #9650, .F. ) ;
#8469 = CARTESIAN_POINT ( 'NONE',  ( -225.0466868817139812, 144.0327468735696073, 6.738601623737560331 ) ) ;
#8470 = ORIENTED_EDGE ( 'NONE', *, *, #1796, .F. ) ;
#8471 = EDGE_CURVE ( 'NONE', #4243, #11151, #10553, .T. ) ;
#8472 = VERTEX_POINT ( 'NONE', #14173 ) ;
#8473 = DIRECTION ( 'NONE',  ( 0.000000000000000000, 0.000000000000000000, 1.000000000000000000 ) ) ;
#8474 = AXIS2_PLACEMENT_3D ( 'NONE', #2313, #14223, #14455 ) ;
#8475 = ORIENTED_EDGE ( 'NONE', *, *, #2911, .T. ) ;
#8476 = DIRECTION ( 'NONE',  ( 0.000000000000000000, 0.000000000000000000, -1.000000000000000000 ) ) ;
#8477 = FACE_OUTER_BOUND ( 'NONE', #14987, .T. ) ;
#8478 = CARTESIAN_POINT ( 'NONE',  ( -110.0000000000000426, 22.53993994372673981, 13.00000000000000178 ) ) ;
#8479 = CIRCLE ( 'NONE', #1146, 5.000000000000017764 ) ;
#8480 = ORIENTED_EDGE ( 'NONE', *, *, #13174, .F. ) ;
#8481 = EDGE_CURVE ( 'NONE', #6899, #411, #11709, .T. ) ;
#8482 = FACE_OUTER_BOUND ( 'NONE', #11125, .T. ) ;
#8483 = EDGE_CURVE ( 'NONE', #2454, #552, #1864, .T. ) ;
#8484 = ORIENTED_EDGE ( 'NONE', *, *, #6451, .T. ) ;
#8485 = AXIS2_PLACEMENT_3D ( 'NONE', #11883, #15489, #13199 ) ;
#8486 = CARTESIAN_POINT ( 'NONE',  ( 114.0000000000000426, 15.03993994372673981, 10.05257423913146475 ) ) ;
#8487 = DIRECTION ( 'NONE',  ( 0.8731965799097685110, -0.4873681696970816879, -0.000000000000000000 ) ) ;
#8488 = CARTESIAN_POINT ( 'NONE',  ( -151.2997148267479020, 108.2756510478057947, -4.950241352008081464 ) ) ;
#8489 = EDGE_LOOP ( 'NONE', ( #5974, #2389, #6035, #3908 ) ) ;
#8490 = ORIENTED_EDGE ( 'NONE', *, *, #2938, .T. ) ;
#8491 = CARTESIAN_POINT ( 'NONE',  ( -193.7157043470890301, 142.0697917816768836, 1.515441477536284332 ) ) ;
#8492 = CARTESIAN_POINT ( 'NONE',  ( 201.4161383703745400, 32.18800505576257365, -3.749910732146560122 ) ) ;
#8493 = EDGE_LOOP ( 'NONE', ( #6487, #12168 ) ) ;
#8494 = FACE_BOUND ( 'NONE', #2180, .T. ) ;
#8495 = DIRECTION ( 'NONE',  ( 0.000000000000000000, 1.000000000000000000, 0.000000000000000000 ) ) ;
#8496 = AXIS2_PLACEMENT_3D ( 'NONE', #10368, #12489, #15162 ) ;
#8497 = CYLINDRICAL_SURFACE ( 'NONE', #11090, 0.4999999999999996114 ) ;
#8498 = EDGE_CURVE ( 'NONE', #7984, #6369, #9299, .T. ) ;
#8499 = VERTEX_POINT ( 'NONE', #3209 ) ;
#8500 = CARTESIAN_POINT ( 'NONE',  ( 205.4081958545874613, 47.87064854543508829, -4.057643371672452481 ) ) ;
#8501 = ORIENTED_EDGE ( 'NONE', *, *, #15293, .F. ) ;
#8502 = CARTESIAN_POINT ( 'NONE',  ( -110.0000000000000426, 19.53993994372674337, 9.999999999999998224 ) ) ;
#8503 = CARTESIAN_POINT ( 'NONE',  ( -76.00000000000001421, -178.8753867012115961, -29.82329228561640022 ) ) ;
#8504 = CARTESIAN_POINT ( 'NONE',  ( -209.2375803003894532, 133.3242992996629539, -0.4555467707853204096 ) ) ;
#8505 = DIRECTION ( 'NONE',  ( 0.000000000000000000, 0.000000000000000000, 1.000000000000000000 ) ) ;
#8506 = ORIENTED_EDGE ( 'NONE', *, *, #10393, .T. ) ;
#8507 = CARTESIAN_POINT ( 'NONE',  ( -218.3193879687431433, 147.6986783750013217, 10.16010209732750980 ) ) ;
#8508 = DIRECTION ( 'NONE',  ( 0.000000000000000000, 0.9902680687415712502, 0.1391731009600584990 ) ) ;
#8509 = ORIENTED_EDGE ( 'NONE', *, *, #3722, .T. ) ;
#8510 = ORIENTED_EDGE ( 'NONE', *, *, #8288, .T. ) ;
#8511 = CARTESIAN_POINT ( 'NONE',  ( -179.4907066695405717, 117.5900258420264350, 2.301225212616437865 ) ) ;
#8512 = DIRECTION ( 'NONE',  ( -0.000000000000000000, 1.000000000000000000, -0.000000000000000000 ) ) ;
#8513 = DIRECTION ( 'NONE',  ( 1.000000000000000000, -0.000000000000000000, -0.000000000000000000 ) ) ;
#8514 = CARTESIAN_POINT ( 'NONE',  ( 164.0000000000000568, 64.51493994372674479, 15.00000000000000355 ) ) ;
#8515 = ADVANCED_FACE ( 'NONE', ( #987 ), #15198, .T. ) ;
#8516 = CARTESIAN_POINT ( 'NONE',  ( -225.5942063258246719, 143.0517798435176360, 0.6110505370848023921 ) ) ;
#8517 = CARTESIAN_POINT ( 'NONE',  ( 170.6368569633305583, 57.90162049975850067, -0.9107274384406883749 ) ) ;
#8518 = CARTESIAN_POINT ( 'NONE',  ( -155.6477983077465410, 110.1970436846185066, 9.719846845941789937 ) ) ;
#8519 = CARTESIAN_POINT ( 'NONE',  ( -63.50000000000002842, 17.53993994372673271, 52.49999999999997868 ) ) ;
#8520 = FACE_OUTER_BOUND ( 'NONE', #148, .T. ) ;
#8521 = ORIENTED_EDGE ( 'NONE', *, *, #10550, .T. ) ;
#8522 = LINE ( 'NONE', #119, #14872 ) ;
#8523 = ORIENTED_EDGE ( 'NONE', *, *, #9809, .F. ) ;
#8524 = DIRECTION ( 'NONE',  ( -1.000000000000000000, 0.000000000000000000, 0.000000000000000000 ) ) ;
#8525 = VECTOR ( 'NONE', #13615, 1000.000000000000000 ) ;
#8526 = DIRECTION ( 'NONE',  ( 0.4873681696970831312, 0.8731965799097676229, 0.000000000000000000 ) ) ;
#8527 = DIRECTION ( 'NONE',  ( 0.000000000000000000, 0.000000000000000000, -1.000000000000000000 ) ) ;
#8528 = PLANE ( 'NONE',  #4968 ) ;
#8529 = DIRECTION ( 'NONE',  ( 0.000000000000000000, 0.000000000000000000, 1.000000000000000000 ) ) ;
#8530 = DIRECTION ( 'NONE',  ( -1.000000000000000000, 0.000000000000000000, 0.000000000000000000 ) ) ;
#8531 = EDGE_CURVE ( 'NONE', #1467, #299, #6860, .T. ) ;
#8532 = ORIENTED_EDGE ( 'NONE', *, *, #4682, .T. ) ;
#8533 = CIRCLE ( 'NONE', #11292, 0.5000000000000004441 ) ;
#8534 = EDGE_CURVE ( 'NONE', #12812, #1838, #6579, .T. ) ;
#8535 = VECTOR ( 'NONE', #14089, 1000.000000000000000 ) ;
#8536 = CARTESIAN_POINT ( 'NONE',  ( 208.7972876766878016, 42.12791357830437988, -6.002605234521809052 ) ) ;
#8537 = DIRECTION ( 'NONE',  ( 0.000000000000000000, -5.551115123125777653E-14, -1.000000000000000000 ) ) ;
#8538 = EDGE_LOOP ( 'NONE', ( #4963, #12010, #7250, #4452 ) ) ;
#8539 = CARTESIAN_POINT ( 'NONE',  ( -220.9079605857687341, 147.3142607384192786, 9.825007490950982358 ) ) ;
#8540 = ORIENTED_EDGE ( 'NONE', *, *, #6824, .T. ) ;
#8541 = DIRECTION ( 'NONE',  ( 1.000000000000000000, 0.000000000000000000, 0.000000000000000000 ) ) ;
#8542 = CARTESIAN_POINT ( 'NONE',  ( 207.3749241153878700, 31.42506699505091916, -7.936699686978753832 ) ) ;
#8543 = VERTEX_POINT ( 'NONE', #3136 ) ;
#8544 = AXIS2_PLACEMENT_3D ( 'NONE', #9108, #5774, #4588 ) ;
#8545 = FACE_OUTER_BOUND ( 'NONE', #15546, .T. ) ;
#8546 = DIRECTION ( 'NONE',  ( 0.8731965799097684000, -0.4873681696970819655, -0.000000000000000000 ) ) ;
#8547 = AXIS2_PLACEMENT_3D ( 'NONE', #13050, #10708, #5810 ) ;
#8548 = EDGE_CURVE ( 'NONE', #12308, #2407, #9586, .T. ) ;
#8549 = CARTESIAN_POINT ( 'NONE',  ( 5.799999999999999822, 4.618802153516981868, -7.999999999999979572 ) ) ;
#8550 = ORIENTED_EDGE ( 'NONE', *, *, #10204, .F. ) ;
#8551 = EDGE_LOOP ( 'NONE', ( #7458, #370 ) ) ;
#8552 = VECTOR ( 'NONE', #12065, 1000.000000000000000 ) ;
#8553 = FACE_OUTER_BOUND ( 'NONE', #5284, .T. ) ;
#8554 = ORIENTED_EDGE ( 'NONE', *, *, #11926, .T. ) ;
#8555 = CARTESIAN_POINT ( 'NONE',  ( 0.000000000000000000, 7.511572993685799101E-16, -2.750000000000000444 ) ) ;
#8556 = CIRCLE ( 'NONE', #3251, 3.525000000000000355 ) ;
#8557 = CARTESIAN_POINT ( 'NONE',  ( -88.79955057502458260, 65.19100426474074084, 10.00000000000000178 ) ) ;
#8558 = ORIENTED_EDGE ( 'NONE', *, *, #7583, .T. ) ;
#8559 = ORIENTED_EDGE ( 'NONE', *, *, #9842, .F. ) ;
#8560 = CARTESIAN_POINT ( 'NONE',  ( -218.6225377568032684, 155.5426184521650441, -0.4568654681747655322 ) ) ;
#8561 = CARTESIAN_POINT ( 'NONE',  ( 208.8060099514817978, 42.07246638764446089, -7.432400171711813996 ) ) ;
#8562 = VERTEX_POINT ( 'NONE', #5593 ) ;
#8563 = ADVANCED_FACE ( 'NONE', ( #2105 ), #6938, .F. ) ;
#8564 = PLANE ( 'NONE',  #14835 ) ;
#8565 = LINE ( 'NONE', #3823, #4950 ) ;
#8566 = EDGE_CURVE ( 'NONE', #1955, #1358, #1766, .T. ) ;
#8567 = ADVANCED_FACE ( 'NONE', ( #12755 ), #11586, .F. ) ;
#8568 = FACE_OUTER_BOUND ( 'NONE', #9007, .T. ) ;
#8569 = AXIS2_PLACEMENT_3D ( 'NONE', #10861, #6199, #11012 ) ;
#8570 = VECTOR ( 'NONE', #13664, 1000.000000000000000 ) ;
#8571 = ORIENTED_EDGE ( 'NONE', *, *, #622, .T. ) ;
#8572 = CARTESIAN_POINT ( 'NONE',  ( -85.99999999999994316, 62.13993994372673768, 15.00000000000174794 ) ) ;
#8573 = CIRCLE ( 'NONE', #7573, 1.700000000000001954 ) ;
#8574 = CARTESIAN_POINT ( 'NONE',  ( 194.7312355367470786, 33.90632498363353164, -3.989214208820068386 ) ) ;
#8575 = ORIENTED_EDGE ( 'NONE', *, *, #1310, .T. ) ;
#8576 = DIRECTION ( 'NONE',  ( -0.000000000000000000, -0.000000000000000000, 1.000000000000000000 ) ) ;
#8577 = CARTESIAN_POINT ( 'NONE',  ( -63.50000000000002842, 16.03993994372673981, 10.05257423913146475 ) ) ;
#8578 = VECTOR ( 'NONE', #5869, 999.9999999999998863 ) ;
#8579 = CARTESIAN_POINT ( 'NONE',  ( -203.7063805325860812, 135.3711971156951677, -4.642206099735014746 ) ) ;
#8580 = AXIS2_PLACEMENT_3D ( 'NONE', #3178, #2363, #796 ) ;
#8581 = CARTESIAN_POINT ( 'NONE',  ( 51.07686401294030532, 368.7106150007013525, 5.000000000000000000 ) ) ;
#8582 = EDGE_LOOP ( 'NONE', ( #6112, #490, #12473, #666 ) ) ;
#8583 = CARTESIAN_POINT ( 'NONE',  ( -205.6684400016210645, 139.7560197894119085, 10.16010209732751157 ) ) ;
#8584 = CARTESIAN_POINT ( 'NONE',  ( 194.7891036845171300, 47.85977741052224133, -6.433373108600371815 ) ) ;
#8585 = VERTEX_POINT ( 'NONE', #2419 ) ;
#8586 = VERTEX_POINT ( 'NONE', #14324 ) ;
#8587 = CARTESIAN_POINT ( 'NONE',  ( -199.4123279565619100, 127.6180083311870845, 2.431555724346860181 ) ) ;
#8588 = CARTESIAN_POINT ( 'NONE',  ( 190.5000000000000853, 16.03993994372673626, 52.49999999999997868 ) ) ;
#8589 = CARTESIAN_POINT ( 'NONE',  ( -85.99999999999994316, 56.53993994372675047, 16.70000000000174012 ) ) ;
#8590 = FACE_BOUND ( 'NONE', #12424, .T. ) ;
#8591 = VECTOR ( 'NONE', #9767, 1000.000000000000000 ) ;
#8592 = CARTESIAN_POINT ( 'NONE',  ( -223.5918188539070002, 142.0538562971642307, 1.612306317632525410 ) ) ;
#8593 = CONICAL_SURFACE ( 'NONE', #6324, 4.172000000000013920, 0.7853981633974430610 ) ;
#8594 = DIRECTION ( 'NONE',  ( 0.000000000000000000, 0.000000000000000000, -1.000000000000000000 ) ) ;
#8595 = FACE_OUTER_BOUND ( 'NONE', #2980, .T. ) ;
#8596 = CIRCLE ( 'NONE', #10358, 3.500000000000004885 ) ;
#8597 = DIRECTION ( 'NONE',  ( 0.000000000000000000, -0.9902680687415712502, -0.1391731009600584990 ) ) ;
#8598 = ORIENTED_EDGE ( 'NONE', *, *, #5870, .T. ) ;
#8599 = VECTOR ( 'NONE', #9740, 1000.000000000000000 ) ;
#8600 = EDGE_CURVE ( 'NONE', #1731, #4058, #12735, .T. ) ;
#8601 = ORIENTED_EDGE ( 'NONE', *, *, #335, .F. ) ;
#8602 = CARTESIAN_POINT ( 'NONE',  ( -110.0000000000000426, 19.53993994372674337, 9.999999999999998224 ) ) ;
#8603 = CARTESIAN_POINT ( 'NONE',  ( 203.4093511297050725, 50.30250970312702208, -0.9107274384406883749 ) ) ;
#8604 = DIRECTION ( 'NONE',  ( 1.000000000000000000, 0.000000000000000000, 0.000000000000000000 ) ) ;
#8605 = DIRECTION ( 'NONE',  ( 0.000000000000000000, -4.956352788505162775E-17, 1.000000000000000000 ) ) ;
#8606 = DIRECTION ( 'NONE',  ( 1.000000000000000000, 0.000000000000000000, 0.000000000000000000 ) ) ;
#8607 = DIRECTION ( 'NONE',  ( -1.000000000000000000, -0.000000000000000000, 0.000000000000000000 ) ) ;
#8608 = LINE ( 'NONE', #7429, #8306 ) ;
#8609 = ORIENTED_EDGE ( 'NONE', *, *, #4340, .F. ) ;
#8610 = AXIS2_PLACEMENT_3D ( 'NONE', #871, #10135, #2949 ) ;
#8611 = EDGE_LOOP ( 'NONE', ( #926, #7760, #13456, #702 ) ) ;
#8612 = CARTESIAN_POINT ( 'NONE',  ( 202.9941614129404286, 48.85583040772959862, -2.484837107663659506 ) ) ;
#8613 = EDGE_CURVE ( 'NONE', #2939, #1838, #13219, .T. ) ;
#8614 = CARTESIAN_POINT ( 'NONE',  ( -219.9178674059391199, 153.2218320532828386, 5.684947844236139858 ) ) ;
#8615 = ORIENTED_EDGE ( 'NONE', *, *, #10464, .F. ) ;
#8616 = CARTESIAN_POINT ( 'NONE',  ( -223.9524810574280593, 145.9931883691309622, 6.118258866120367401 ) ) ;
#8617 = ORIENTED_EDGE ( 'NONE', *, *, #9049, .F. ) ;
#8618 = LINE ( 'NONE', #4982, #8798 ) ;
#8619 = CARTESIAN_POINT ( 'NONE',  ( 188.3013221956022392, 42.41630894433524190, -3.062925739686887638 ) ) ;
#8620 = VECTOR ( 'NONE', #9546, 1000.000000000000000 ) ;
#8621 = ORIENTED_EDGE ( 'NONE', *, *, #3920, .F. ) ;
#8622 = DIRECTION ( 'NONE',  ( 1.000000000000000000, 0.000000000000000000, 0.000000000000000000 ) ) ;
#8623 = DIRECTION ( 'NONE',  ( 0.000000000000000000, -1.000000000000000000, 0.000000000000000000 ) ) ;
#8624 = EDGE_CURVE ( 'NONE', #8197, #8640, #11603, .T. ) ;
#8625 = CYLINDRICAL_SURFACE ( 'NONE', #2085, 1.700000000000000178 ) ;
#8626 = VERTEX_POINT ( 'NONE', #6435 ) ;
#8627 = AXIS2_PLACEMENT_3D ( 'NONE', #9287, #14084, #3285 ) ;
#8628 = ORIENTED_EDGE ( 'NONE', *, *, #7640, .F. ) ;
#8629 = CYLINDRICAL_SURFACE ( 'NONE', #14964, 1.700000000000007061 ) ;
#8630 = AXIS2_PLACEMENT_3D ( 'NONE', #12385, #9794, #6326 ) ;
#8631 = DIRECTION ( 'NONE',  ( -1.000000000000000000, 0.000000000000000000, 0.000000000000000000 ) ) ;
#8632 = VERTEX_POINT ( 'NONE', #10796 ) ;
#8633 = CARTESIAN_POINT ( 'NONE',  ( 163.3793289068652541, 15.80605437029534954, -6.370175303308202253 ) ) ;
#8634 = EDGE_CURVE ( 'NONE', #3314, #4605, #14408, .T. ) ;
#8635 = FACE_OUTER_BOUND ( 'NONE', #13922, .T. ) ;
#8636 = EDGE_LOOP ( 'NONE', ( #11622, #5922, #12878, #175 ) ) ;
#8637 = VERTEX_POINT ( 'NONE', #10956 ) ;
#8638 = CARTESIAN_POINT ( 'NONE',  ( -170.0916760340589349, 128.4977246429275226, -0.4609024664951656969 ) ) ;
#8639 = CARTESIAN_POINT ( 'NONE',  ( 194.7891036845171300, 47.85977741052224133, -6.433373108600371815 ) ) ;
#8640 = VERTEX_POINT ( 'NONE', #3523 ) ;
#8641 = COLOUR_RGB ( '', 0.40784314, 0.44705882, 0.49803922) ;
#8642 = CARTESIAN_POINT ( 'NONE',  ( -157.5453996073046881, 109.6804705170678034, -4.377525546821591007 ) ) ;
#8643 = CARTESIAN_POINT ( 'NONE',  ( -76.00000000000001421, -178.8058001507315566, -30.31842631998718574 ) ) ;
#8645 = AXIS2_PLACEMENT_3D ( 'NONE', #1323, #8379, #13317 ) ;
#8644 = CIRCLE ( 'NONE', #9910, 1.699999999999998401 ) ;
#8646 = CARTESIAN_POINT ( 'NONE',  ( -63.50000000000002842, 15.53993994372673981, -3.075184203610571654 ) ) ;
#8647 = EDGE_CURVE ( 'NONE', #12461, #10711, #2583, .T. ) ;
#8648 = SHAPE_REPRESENTATION ( 'Cast Iron Frame Side Blocks x2', ( #12337 ), #180 ) ;
#8649 = LINE ( 'NONE', #9912, #12156 ) ;
#8650 = CARTESIAN_POINT ( 'NONE',  ( 208.7983505906672121, 39.57879239708907448, -2.990627279509298742 ) ) ;
#8651 = VERTEX_POINT ( 'NONE', #4948 ) ;
#8652 = DIRECTION ( 'NONE',  ( 0.000000000000000000, 1.000000000000000000, 6.938893903907227145E-17 ) ) ;
#8653 = LINE ( 'NONE', #3186, #2403 ) ;
#8654 = CARTESIAN_POINT ( 'NONE',  ( -208.3893201713671033, 134.8533518211819739, -2.964974570226836192 ) ) ;
#8656 = ADVANCED_FACE ( 'NONE', ( #8360 ), #106, .F. ) ;
#8655 = PLANE ( 'NONE',  #960 ) ;
#8657 = EDGE_CURVE ( 'NONE', #15235, #6079, #14555, .T. ) ;
#8658 = ORIENTED_EDGE ( 'NONE', *, *, #2545, .T. ) ;
#8659 = CARTESIAN_POINT ( 'NONE',  ( -177.0244624812495999, 127.4802545373068767, 9.556866313350486308 ) ) ;
#8660 = CONICAL_SURFACE ( 'NONE', #10668, 3.525000000000000355, 0.7853981633974482790 ) ;
#8661 = CARTESIAN_POINT ( 'NONE',  ( 201.2658342953964166, 49.58143373454755931, -3.806719548689701416 ) ) ;
#8662 = ORIENTED_EDGE ( 'NONE', *, *, #5038, .F. ) ;
#8663 = ORIENTED_EDGE ( 'NONE', *, *, #4851, .T. ) ;
#8664 = EDGE_CURVE ( 'NONE', #14199, #9410, #14371, .T. ) ;
#8665 = VECTOR ( 'NONE', #6233, 1000.000000000000000 ) ;
#8666 = CARTESIAN_POINT ( 'NONE',  ( 175.9483885134608272, -179.3058001507315566, 52.76585208085545275 ) ) ;
#8667 = LINE ( 'NONE', #13459, #7484 ) ;
#8668 = CARTESIAN_POINT ( 'NONE',  ( -86.77455057502459113, 65.19100426474074084, 5.000000000000000000 ) ) ;
#8669 = CARTESIAN_POINT ( 'NONE',  ( -35.99999999999995026, 64.53993994372673626, 15.00000000000139977 ) ) ;
#8670 = CARTESIAN_POINT ( 'NONE',  ( 178.0000000000000853, 15.53993994372673981, -17.50000000000002487 ) ) ;
#8671 = EDGE_CURVE ( 'NONE', #830, #9239, #9690, .T. ) ;
#8673 = ADVANCED_FACE ( 'NONE', ( #7176 ), #11350, .T. ) ;
#8672 =( REPRESENTATION_RELATIONSHIP ('NONE','NONE', #3298, #12546 ) REPRESENTATION_RELATIONSHIP_WITH_TRANSFORMATION ( #861 )SHAPE_REPRESENTATION_RELATIONSHIP( ) );
#8674 = CARTESIAN_POINT ( 'NONE',  ( -180.9926919874575333, 132.4923963613727267, 7.919662025281893669 ) ) ;
#8675 = CARTESIAN_POINT ( 'NONE',  ( 6.800000000000000711, 0.000000000000000000, 5.000000000000000000 ) ) ;
#8676 = DIRECTION ( 'NONE',  ( -1.000000000000000000, 0.000000000000000000, 0.000000000000000000 ) ) ;
#8677 = ORIENTED_EDGE ( 'NONE', *, *, #1163, .F. ) ;
#8678 = DIRECTION ( 'NONE',  ( 0.000000000000000000, 0.000000000000000000, -1.000000000000000000 ) ) ;
#8679 = EDGE_LOOP ( 'NONE', ( #2418, #1219 ) ) ;
#8680 = LINE ( 'NONE', #6309, #4997 ) ;
#8681 = DIRECTION ( 'NONE',  ( -0.000000000000000000, -0.000000000000000000, 1.000000000000000000 ) ) ;
#8682 = CIRCLE ( 'NONE', #2110, 4.499999999999950262 ) ;
#8683 = CARTESIAN_POINT ( 'NONE',  ( 190.5000000000000568, 19.53993994372674337, 24.99999999999999645 ) ) ;
#8684 = DIRECTION ( 'NONE',  ( -1.000000000000000000, -0.000000000000000000, -0.000000000000000000 ) ) ;
#8685 = CARTESIAN_POINT ( 'NONE',  ( -35.99999999999995026, 64.53993994372673626, 15.00000000000139977 ) ) ;
#8686 = CARTESIAN_POINT ( 'NONE',  ( 177.5000000000000853, -179.8058001507315566, -30.31842631998718574 ) ) ;
#8687 = CARTESIAN_POINT ( 'NONE',  ( -193.1820620331849341, 139.2949851078578831, 7.919662025281897222 ) ) ;
#8688 = CIRCLE ( 'NONE', #12946, 1.700000000000000178 ) ;
#8689 = ORIENTED_EDGE ( 'NONE', *, *, #1281, .T. ) ;
#8690 = EDGE_CURVE ( 'NONE', #3509, #9250, #2260, .T. ) ;
#8691 = CARTESIAN_POINT ( 'NONE',  ( 17.41029453487719181, 40.04259805664093363, 10.00000000000000178 ) ) ;
#8692 = AXIS2_PLACEMENT_3D ( 'NONE', #13151, #13390, #7103 ) ;
#8693 = CARTESIAN_POINT ( 'NONE',  ( -76.00000000000001421, 16.03993994372673981, -17.50000000000002487 ) ) ;
#8694 = CARTESIAN_POINT ( 'NONE',  ( -220.2512114020426850, 152.6245939580821300, 6.492172721524804402 ) ) ;
#8695 = ORIENTED_EDGE ( 'NONE', *, *, #13511, .F. ) ;
#8696 = CARTESIAN_POINT ( 'NONE',  ( -220.1311302832748424, 152.8397381319110480, 6.240814112616865472 ) ) ;
#8697 = VERTEX_POINT ( 'NONE', #1597 ) ;
#8698 = CARTESIAN_POINT ( 'NONE',  ( -167.9692492009162663, 127.2893952669590902, -0.01570012775376914554 ) ) ;
#8699 = CARTESIAN_POINT ( 'NONE',  ( 201.6484243246164851, 29.05774458226736812, -5.195439731742398592 ) ) ;
#8700 = EDGE_LOOP ( 'NONE', ( #7387, #7514, #13742, #4479 ) ) ;
#8701 = LINE ( 'NONE', #5519, #4136 ) ;
#8702 = CARTESIAN_POINT ( 'NONE',  ( -35.99999999999995026, 56.53993994372675047, 13.30000000000139870 ) ) ;
#8703 = CIRCLE ( 'NONE', #13987, 3.525000000000000355 ) ;
#8704 = CYLINDRICAL_SURFACE ( 'NONE', #5107, 0.5000000000000000000 ) ;
#8705 = EDGE_LOOP ( 'NONE', ( #1751, #9941, #4537, #10470 ) ) ;
#8706 =( NAMED_UNIT ( * ) PLANE_ANGLE_UNIT ( ) SI_UNIT ( $, .RADIAN. ) );
#8707 = ORIENTED_EDGE ( 'NONE', *, *, #13225, .F. ) ;
#8708 = DIRECTION ( 'NONE',  ( -0.000000000000000000, 1.000000000000000000, -0.000000000000000000 ) ) ;
#8709 = CARTESIAN_POINT ( 'NONE',  ( -155.6477983077465410, 110.1970436846185066, 9.719846845941789937 ) ) ;
#8710 = ORIENTED_EDGE ( 'NONE', *, *, #11002, .T. ) ;
#8711 = DIRECTION ( 'NONE',  ( 0.000000000000000000, 0.000000000000000000, 1.000000000000000000 ) ) ;
#8712 = AXIS2_PLACEMENT_3D ( 'NONE', #10299, #6830, #11642 ) ;
#8713 = DIRECTION ( 'NONE',  ( 0.000000000000000000, 1.000000000000000000, 0.000000000000000000 ) ) ;
#8714 = EDGE_LOOP ( 'NONE', ( #5489, #3676, #8957, #612 ) ) ;
#8715 = ORIENTED_EDGE ( 'NONE', *, *, #436, .T. ) ;
#8716 = LINE ( 'NONE', #7533, #2741 ) ;
#8717 = CARTESIAN_POINT ( 'NONE',  ( 202.8882743124338504, 32.81631024066724933, -8.087096619718394663 ) ) ;
#8718 = ORIENTED_EDGE ( 'NONE', *, *, #8923, .T. ) ;
#8719 = DIRECTION ( 'NONE',  ( -3.965082230804130220E-16, 1.090924371466202084E-47, 1.000000000000000000 ) ) ;
#8720 = DIRECTION ( 'NONE',  ( -0.000000000000000000, -0.000000000000000000, 1.000000000000000000 ) ) ;
#8721 = AXIS2_PLACEMENT_3D ( 'NONE', #8633, #231, #14689 ) ;
#8722 = EDGE_CURVE ( 'NONE', #5154, #10184, #13291, .T. ) ;
#8723 = AXIS2_PLACEMENT_3D ( 'NONE', #9748, #11010, #7622 ) ;
#8724 = DIRECTION ( 'NONE',  ( -0.000000000000000000, -0.9902680687415712502, -0.1391731009600586100 ) ) ;
#8725 = CARTESIAN_POINT ( 'NONE',  ( 207.2666510146856069, 31.35441966018789728, -3.370316356820458381 ) ) ;
#8726 = ORIENTED_EDGE ( 'NONE', *, *, #2736, .T. ) ;
#8727 = DIRECTION ( 'NONE',  ( 1.000000000000000000, -0.000000000000000000, -0.000000000000000000 ) ) ;
#8728 = CARTESIAN_POINT ( 'NONE',  ( -216.8024222916085932, 154.7089832689310640, 0.6433992783599493670 ) ) ;
#8729 = CARTESIAN_POINT ( 'NONE',  ( -175.8505196906716890, 123.8775902107358036, -5.297343846388533173 ) ) ;
#8730 = DIRECTION ( 'NONE',  ( 1.000000000000000000, 0.000000000000000000, 0.000000000000000000 ) ) ;
#8731 = VERTEX_POINT ( 'NONE', #13913 ) ;
#8732 = CARTESIAN_POINT ( 'NONE',  ( -191.3393351389284192, 126.0399454915928317, 5.434137442415923225 ) ) ;
#8733 = CARTESIAN_POINT ( 'NONE',  ( 194.7691866843436799, 33.87697957786221536, -2.559886773443665220 ) ) ;
#8734 = ORIENTED_EDGE ( 'NONE', *, *, #1797, .F. ) ;
#8735 = ORIENTED_EDGE ( 'NONE', *, *, #6340, .T. ) ;
#8736 = EDGE_CURVE ( 'NONE', #10088, #5037, #8009, .T. ) ;
#8737 = CIRCLE ( 'NONE', #13263, 3.525000000000000355 ) ;
#8738 = CARTESIAN_POINT ( 'NONE',  ( 184.0000000000000568, 19.53993994372674337, -12.49999999999999467 ) ) ;
#8739 = DIRECTION ( 'NONE',  ( 0.000000000000000000, 0.5000000000000018874, 0.8660254037844375974 ) ) ;
#8740 = DIRECTION ( 'NONE',  ( -0.000000000000000000, 0.000000000000000000, -1.000000000000000000 ) ) ;
#8741 = EDGE_CURVE ( 'NONE', #13912, #9198, #5803, .T. ) ;
#8742 = CARTESIAN_POINT ( 'NONE',  ( 178.0000000000000853, -179.8058001507315566, 52.49999999999997868 ) ) ;
#8743 = EDGE_CURVE ( 'NONE', #10266, #8392, #15545, .T. ) ;
#8744 = DIRECTION ( 'NONE',  ( -1.000000000000000000, 0.000000000000000000, 0.000000000000000000 ) ) ;
#8745 = CARTESIAN_POINT ( 'NONE',  ( -202.9262818645171649, 144.6968105762408072, 7.919662025281898998 ) ) ;
#8746 = DIRECTION ( 'NONE',  ( 1.000000000000000000, 0.000000000000000000, 0.000000000000000000 ) ) ;
#8747 = LINE ( 'NONE', #3689, #10397 ) ;
#8748 = EDGE_LOOP ( 'NONE', ( #14383, #9016, #739, #7604 ) ) ;
#8749 = DIRECTION ( 'NONE',  ( 0.000000000000000000, 4.956352788505162775E-17, -1.000000000000000000 ) ) ;
#8750 = ORIENTED_EDGE ( 'NONE', *, *, #731, .T. ) ;
#8751 = VERTEX_POINT ( 'NONE', #3104 ) ;
#8752 = CARTESIAN_POINT ( 'NONE',  ( -150.4347051859938915, 107.5351962207867871, 9.769471784547334892 ) ) ;
#8753 = CARTESIAN_POINT ( 'NONE',  ( 6.399999999999999467, 9.237604307034018802, 0.000000000000000000 ) ) ;
#8754 = DIRECTION ( 'NONE',  ( 5.518327896226364679E-17, -0.9902680687415713612, 0.1391731009600582492 ) ) ;
#8755 = DIRECTION ( 'NONE',  ( 1.000000000000000000, 0.000000000000000000, 0.000000000000000000 ) ) ;
#8756 = CARTESIAN_POINT ( 'NONE',  ( 17.41029453487719181, 40.04259805664093363, 5.000000000000000000 ) ) ;
#8757 = LINE ( 'NONE', #3863, #8836 ) ;
#8758 = CARTESIAN_POINT ( 'NONE',  ( -174.9866660642990155, 131.1312866983521701, 5.432615396193912538 ) ) ;
#8759 = ADVANCED_FACE ( 'NONE', ( #11633 ), #4029, .T. ) ;
#8760 = EDGE_CURVE ( 'NONE', #4694, #8543, #7697, .T. ) ;
#8761 = EDGE_CURVE ( 'NONE', #10463, #14752, #13884, .T. ) ;
#8762 = ORIENTED_EDGE ( 'NONE', *, *, #7985, .F. ) ;
#8763 = CARTESIAN_POINT ( 'NONE',  ( 201.2541767070109984, 32.14103196098812987, -5.186035738131804962 ) ) ;
#8764 = CARTESIAN_POINT ( 'NONE',  ( -220.5182597048680577, 152.1461350040581806, 6.948896239284471754 ) ) ;
#8765 = ORIENTED_EDGE ( 'NONE', *, *, #10324, .F. ) ;
#8766 = CARTESIAN_POINT ( 'NONE',  ( -218.7722506038294341, 155.2743843858097534, 5.584835994200316733 ) ) ;
#8767 = EDGE_LOOP ( 'NONE', ( #4191, #5547 ) ) ;
#8768 = CARTESIAN_POINT ( 'NONE',  ( -139.1458939983161827, 103.0129948961282054, 2.431557144026069928 ) ) ;
#8769 = CARTESIAN_POINT ( 'NONE',  ( -85.99999999999994316, 64.53993994372673626, 11.47500000000174758 ) ) ;
#8770 = ADVANCED_FACE ( 'NONE', ( #10336 ), #13875, .T. ) ;
#8771 = VERTEX_POINT ( 'NONE', #12689 ) ;
#8772 = CYLINDRICAL_SURFACE ( 'NONE', #4105, 3.500000000000003109 ) ;
#8773 = DIRECTION ( 'NONE',  ( 1.000000000000000000, 0.000000000000000000, 0.000000000000000000 ) ) ;
#8774 = CIRCLE ( 'NONE', #2221, 0.4999999999999998890 ) ;
#8775 = CARTESIAN_POINT ( 'NONE',  ( 184.0000000000000568, 17.53993994372673981, -12.49999999999999289 ) ) ;
#8776 = ORIENTED_EDGE ( 'NONE', *, *, #14212, .T. ) ;
#8777 = AXIS2_PLACEMENT_3D ( 'NONE', #1819, #6662, #8867 ) ;
#8778 = CARTESIAN_POINT ( 'NONE',  ( -70.00000000000000000, 21.53993994372674337, -12.49999999999999645 ) ) ;
#8779 = ORIENTED_EDGE ( 'NONE', *, *, #10114, .F. ) ;
#8780 = CARTESIAN_POINT ( 'NONE',  ( 64.00000000000005684, 64.53993994372673626, 13.30000000000070948 ) ) ;
#8781 = CARTESIAN_POINT ( 'NONE',  ( -157.5298637219052296, 110.6847670947880573, 9.583914075210627104 ) ) ;
#8782 = ORIENTED_EDGE ( 'NONE', *, *, #13150, .T. ) ;
#8783 = FACE_BOUND ( 'NONE', #6391, .T. ) ;
#8784 = CIRCLE ( 'NONE', #1963, 0.4999999999999998890 ) ;
#8785 = EDGE_CURVE ( 'NONE', #9678, #13452, #9234, .T. ) ;
#8786 = EDGE_CURVE ( 'NONE', #12099, #470, #13356, .T. ) ;
#8787 = CARTESIAN_POINT ( 'NONE',  ( 5.799999999999999822, 7.999999999999979572, 0.000000000000000000 ) ) ;
#8788 = ORIENTED_EDGE ( 'NONE', *, *, #3081, .F. ) ;
#8789 = VERTEX_POINT ( 'NONE', #5678 ) ;
#8790 = CARTESIAN_POINT ( 'NONE',  ( 172.5293059057019889, 61.25683321636181233, 5.000000000000000000 ) ) ;
#8791 = CARTESIAN_POINT ( 'NONE',  ( 202.9941614129404286, 48.85583040772959862, -2.484837107663659506 ) ) ;
#8792 = CIRCLE ( 'NONE', #14562, 0.5000000000000004441 ) ;
#8793 = EDGE_CURVE ( 'NONE', #10245, #2490, #14032, .T. ) ;
#8794 = VERTEX_POINT ( 'NONE', #5445 ) ;
#8795 = CARTESIAN_POINT ( 'NONE',  ( -157.2597666735746031, 109.3947789516118405, -4.325135862343416626 ) ) ;
#8796 = DIRECTION ( 'NONE',  ( -0.8660254037844387076, -0.5000000000000001110, 0.000000000000000000 ) ) ;
#8797 = DIRECTION ( 'NONE',  ( 0.000000000000000000, 0.000000000000000000, 1.000000000000000000 ) ) ;
#8798 = VECTOR ( 'NONE', #1337, 1000.000000000000000 ) ;
#8799 = AXIS2_PLACEMENT_3D ( 'NONE', #9456, #9379, #2182 ) ;
#8800 = ORIENTED_EDGE ( 'NONE', *, *, #12696, .T. ) ;
#8801 = CIRCLE ( 'NONE', #7299, 17.06579782980005433 ) ;
#8802 = AXIS2_PLACEMENT_3D ( 'NONE', #3671, #9845, #9919 ) ;
#8803 = DIRECTION ( 'NONE',  ( 0.000000000000000000, 0.000000000000000000, 1.000000000000000000 ) ) ;
#8804 = ORIENTED_EDGE ( 'NONE', *, *, #2804, .F. ) ;
#8805 = CARTESIAN_POINT ( 'NONE',  ( -222.2781198963554061, 144.6180712093748753, -3.576421514447124750 ) ) ;
#8806 = CARTESIAN_POINT ( 'NONE',  ( -210.8320337336493822, 142.3623933791497791, -5.230826428279598872 ) ) ;
#8807 = LINE ( 'NONE', #1841, #10567 ) ;
#8808 = VERTEX_POINT ( 'NONE', #1950 ) ;
#8809 = CARTESIAN_POINT ( 'NONE',  ( -218.1518098834511648, 139.2461763302102327, 3.478895870929506362 ) ) ;
#8810 = CARTESIAN_POINT ( 'NONE',  ( 194.7312355367470786, 33.90632498363353164, -3.989214208820068386 ) ) ;
#8811 = VERTEX_POINT ( 'NONE', #10259 ) ;
#8812 = AXIS2_PLACEMENT_3D ( 'NONE', #8768, #12389, #5289 ) ;
#8813 = CIRCLE ( 'NONE', #1991, 1.499999999999999778 ) ;
#8814 = CARTESIAN_POINT ( 'NONE',  ( 0.06809871960543052716, -6.146186931204450588, -5.354491962338080668 ) ) ;
#8815 = CARTESIAN_POINT ( 'NONE',  ( 2.000000000000000000, -3.175426480542940411, 0.000000000000000000 ) ) ;
#8816 = ADVANCED_FACE ( 'NONE', ( #11681, #11521, #11756, #15049, #9081, #679, #9313, #844, #5523, #3382 ), #4477, .T. ) ;
#8817 = DIRECTION ( 'NONE',  ( 0.000000000000000000, 1.000000000000000000, 0.000000000000000000 ) ) ;
#8818 = MECHANICAL_DESIGN_GEOMETRIC_PRESENTATION_REPRESENTATION (  '', ( #5355 ), #14346 ) ;
#8819 = LINE ( 'NONE', #11263, #78 ) ;
#8820 = EDGE_CURVE ( 'NONE', #15257, #7752, #753, .T. ) ;
#8821 = AXIS2_PLACEMENT_3D ( 'NONE', #5709, #7938, #3339 ) ;
#8822 = CARTESIAN_POINT ( 'NONE',  ( -70.00000000000000000, 19.53993994372673626, 47.49999999999997868 ) ) ;
#8823 = CARTESIAN_POINT ( 'NONE',  ( -172.3625742532922800, 130.1311808564658747, 3.478855110039204224 ) ) ;
#8824 = FACE_OUTER_BOUND ( 'NONE', #1710, .T. ) ;
#8825 = LINE ( 'NONE', #6465, #9082 ) ;
#8826 = ORIENTED_EDGE ( 'NONE', *, *, #14111, .F. ) ;
#8827 = DIRECTION ( 'NONE',  ( -3.862829527358613429E-15, -0.9902680687415705840, 0.1391731009600641333 ) ) ;
#8828 = ADVANCED_FACE ( 'NONE', ( #7980 ), #13600, .F. ) ;
#8829 = ORIENTED_EDGE ( 'NONE', *, *, #2529, .T. ) ;
#8830 = ORIENTED_EDGE ( 'NONE', *, *, #11927, .T. ) ;
#8831 = CONICAL_SURFACE ( 'NONE', #1755, 3.525000000000000355, 0.7853981633974482790 ) ;
#8832 = PLANE ( 'NONE',  #7806 ) ;
#8833 = LINE ( 'NONE', #8602, #9037 ) ;
#8834 = AXIS2_PLACEMENT_3D ( 'NONE', #1149, #13296, #7252 ) ;
#8835 = DIRECTION ( 'NONE',  ( -0.000000000000000000, 1.000000000000000000, -0.000000000000000000 ) ) ;
#8836 = VECTOR ( 'NONE', #12377, 1000.000000000000000 ) ;
#8837 = CARTESIAN_POINT ( 'NONE',  ( 14.00000000000004086, 64.53993994372673626, 16.70000000000104734 ) ) ;
#8838 = LINE ( 'NONE', #9947, #13514 ) ;
#8839 = LINE ( 'NONE', #12760, #3274 ) ;
#8840 = CARTESIAN_POINT ( 'NONE',  ( -167.6801169734147265, 127.1165587117766336, 5.426559898713293251 ) ) ;
#8841 = ORIENTED_EDGE ( 'NONE', *, *, #9721, .T. ) ;
#8842 = CARTESIAN_POINT ( 'NONE',  ( 0.1708300674639753880, 1.717253364505211266, -2.525629923208373651 ) ) ;
#8843 = AXIS2_PLACEMENT_3D ( 'NONE', #4744, #8322, #13339 ) ;
#8844 = CIRCLE ( 'NONE', #10864, 1.000000000000000888 ) ;
#8845 = TOROIDAL_SURFACE ( 'NONE', #10352, 21.91351791792154202, 1.499999999999997113 ) ;
#8846 = CARTESIAN_POINT ( 'NONE',  ( 207.1164837741930569, 35.57719129110033407, -1.806778302941847159 ) ) ;
#8847 = DIRECTION ( 'NONE',  ( -0.000000000000000000, -0.000000000000000000, 1.000000000000000000 ) ) ;
#8848 = EDGE_LOOP ( 'NONE', ( #8416, #1297, #9817, #7814, #1969 ) ) ;
#8849 = ADVANCED_FACE ( 'NONE', ( #13963 ), #4563, .T. ) ;
#8850 = CARTESIAN_POINT ( 'NONE',  ( -221.9718704697112059, 149.5417631404425265, 7.948023732481154013 ) ) ;
#8852 = EDGE_CURVE ( 'NONE', #12081, #620, #8347, .T. ) ;
#8851 = EDGE_CURVE ( 'NONE', #9167, #2929, #12767, .T. ) ;
#8853 = ORIENTED_EDGE ( 'NONE', *, *, #3852, .T. ) ;
#8854 = DIRECTION ( 'NONE',  ( 0.000000000000000000, 0.000000000000000000, 1.000000000000000000 ) ) ;
#8855 = CARTESIAN_POINT ( 'NONE',  ( 211.8810731409095922, 42.48823013260103920, -7.441781176392031405 ) ) ;
#8856 = ORIENTED_EDGE ( 'NONE', *, *, #12091, .F. ) ;
#8857 = CARTESIAN_POINT ( 'NONE',  ( -63.50000000000002842, 15.53993994372673981, -17.50000000000002487 ) ) ;
#8858 = CYLINDRICAL_SURFACE ( 'NONE', #7599, 0.4999999999999996114 ) ;
#8859 = VECTOR ( 'NONE', #5533, 999.9999999999998863 ) ;
#8860 = EDGE_CURVE ( 'NONE', #701, #9198, #1083, .T. ) ;
#8861 = TOROIDAL_SURFACE ( 'NONE', #12877, 1.000000000000000000, 0.5000000000000000000 ) ;
#8862 = FACE_OUTER_BOUND ( 'NONE', #1510, .T. ) ;
#8863 = ORIENTED_EDGE ( 'NONE', *, *, #14425, .F. ) ;
#8864 = PRODUCT_CONTEXT ( 'NONE', #9917, 'mechanical' ) ;
#8865 = EDGE_LOOP ( 'NONE', ( #8087, #5641 ) ) ;
#8866 = LINE ( 'NONE', #6500, #4393 ) ;
#8867 = DIRECTION ( 'NONE',  ( 0.000000000000000000, 0.000000000000000000, -1.000000000000000000 ) ) ;
#8868 = ORIENTED_EDGE ( 'NONE', *, *, #12783, .F. ) ;
#8869 = DIRECTION ( 'NONE',  ( 0.000000000000000000, -0.9902680687415713612, 0.1391731009600582492 ) ) ;
#8870 = AXIS2_PLACEMENT_3D ( 'NONE', #10190, #4171, #9010 ) ;
#8871 = EDGE_CURVE ( 'NONE', #7752, #15257, #4792, .T. ) ;
#8872 = PLANE ( 'NONE',  #7059 ) ;
#8873 = VERTEX_POINT ( 'NONE', #6149 ) ;
#8874 = EDGE_LOOP ( 'NONE', ( #8782, #15539, #11389, #2632 ) ) ;
#8875 = DIRECTION ( 'NONE',  ( -0.000000000000000000, -0.000000000000000000, 1.000000000000000000 ) ) ;
#8876 = CARTESIAN_POINT ( 'NONE',  ( 205.4526553411199359, 47.86694802938139759, -2.633259993550844502 ) ) ;
#8877 = VERTEX_POINT ( 'NONE', #13306 ) ;
#8878 = CARTESIAN_POINT ( 'NONE',  ( 207.1131222881253393, 35.56952893079440514, -7.807171136772324438 ) ) ;
#8879 = CARTESIAN_POINT ( 'NONE',  ( 195.1062858801516597, 40.86394065090267702, -20.00000000000000000 ) ) ;
#8880 = EDGE_CURVE ( 'NONE', #14396, #11858, #8371, .T. ) ;
#8881 = CARTESIAN_POINT ( 'NONE',  ( -157.6477983077465410, 109.9391580343927473, -4.459856507254698954 ) ) ;
#8882 = DIRECTION ( 'NONE',  ( -0.000000000000000000, -1.000000000000000000, -0.000000000000000000 ) ) ;
#8883 = CARTESIAN_POINT ( 'NONE',  ( 122.5806775638430253, 45.00321902537314145, 5.000000000000000000 ) ) ;
#8884 = CONICAL_SURFACE ( 'NONE', #6104, 8.000000000000028422, 1.047197551196600296 ) ;
#8885 = APPLICATION_CONTEXT ( 'automotive_design' ) ;
#8886 = CONICAL_SURFACE ( 'NONE', #2059, 3.525000000000000355, 0.7853981633974482790 ) ;
#8887 = ADVANCED_FACE ( 'NONE', ( #46 ), #15439, .F. ) ;
#8888 = DIRECTION ( 'NONE',  ( -0.000000000000000000, 0.000000000000000000, 1.000000000000000000 ) ) ;
#8889 = ORIENTED_EDGE ( 'NONE', *, *, #8657, .F. ) ;
#8890 = DIRECTION ( 'NONE',  ( -0.8731965799097685110, 0.4873681696970816324, 0.000000000000000000 ) ) ;
#8891 = DIRECTION ( 'NONE',  ( -0.000000000000000000, -0.000000000000000000, -1.000000000000000000 ) ) ;
#8892 = CARTESIAN_POINT ( 'NONE',  ( -199.2233958860587961, 127.9753750774359276, -0.4555467707853375070 ) ) ;
#8893 = DIRECTION ( 'NONE',  ( 1.000000000000000000, -2.751328491981765035E-32, 3.965082230804130220E-16 ) ) ;
#8894 = VERTEX_POINT ( 'NONE', #8450 ) ;
#8895 = CARTESIAN_POINT ( 'NONE',  ( -200.9709139173866959, 128.5579952147370761, 5.434137442415933883 ) ) ;
#8897 = CARTESIAN_POINT ( 'NONE',  ( 203.2140370934807834, 48.77700970988914264, -0.9247215889056725757 ) ) ;
#8896 = AXIS2_PLACEMENT_3D ( 'NONE', #10626, #9368, #2094 ) ;
#8898 = EDGE_LOOP ( 'NONE', ( #9441, #14356, #7652, #12872 ) ) ;
#8899 = AXIS2_PLACEMENT_3D ( 'NONE', #4646, #13891, #12698 ) ;
#8900 = DIRECTION ( 'NONE',  ( -3.965082230804130220E-16, 0.000000000000000000, 1.000000000000000000 ) ) ;
#8901 = DIRECTION ( 'NONE',  ( -1.000000000000000000, 0.000000000000000000, 0.000000000000000000 ) ) ;
#8902 = CYLINDRICAL_SURFACE ( 'NONE', #9597, 3.499999999999999556 ) ;
#8903 = ADVANCED_FACE ( 'NONE', ( #15517 ), #5503, .T. ) ;
#8904 = DIRECTION ( 'NONE',  ( 0.000000000000000000, -0.1391731009600586100, 0.9902680687415712502 ) ) ;
#8905 = CIRCLE ( 'NONE', #6132, 1.500000000000000666 ) ;
#8906 = ORIENTED_EDGE ( 'NONE', *, *, #12884, .T. ) ;
#8907 = LINE ( 'NONE', #13698, #5919 ) ;
#8908 = DIRECTION ( 'NONE',  ( 0.000000000000000000, 0.000000000000000000, 1.000000000000000000 ) ) ;
#8909 = DIRECTION ( 'NONE',  ( 0.000000000000000000, 0.000000000000000000, -1.000000000000000000 ) ) ;
#8910 = ORIENTED_EDGE ( 'NONE', *, *, #11356, .F. ) ;
#8911 = AXIS2_PLACEMENT_3D ( 'NONE', #10918, #11146, #7441 ) ;
#8912 = DIRECTION ( 'NONE',  ( 0.000000000000000000, -0.000000000000000000, -1.000000000000000000 ) ) ;
#8913 = ORIENTED_EDGE ( 'NONE', *, *, #7217, .F. ) ;
#8914 = VERTEX_POINT ( 'NONE', #15481 ) ;
#8915 = DIRECTION ( 'NONE',  ( -0.000000000000000000, -0.000000000000000000, 1.000000000000000000 ) ) ;
#8916 = DIRECTION ( 'NONE',  ( -0.000000000000000000, -0.000000000000000000, 1.000000000000000000 ) ) ;
#8917 = DIRECTION ( 'NONE',  ( -0.000000000000000000, -0.000000000000000000, 1.000000000000000000 ) ) ;
#8918 = CARTESIAN_POINT ( 'NONE',  ( 0.2456200930618588907, -1.587713240271461546, 2.750000000000000000 ) ) ;
#8919 = DIRECTION ( 'NONE',  ( -0.000000000000000000, -1.000000000000000000, -0.000000000000000000 ) ) ;
#8920 = CARTESIAN_POINT ( 'NONE',  ( -220.0433514299955391, 152.9970077265409998, -3.801945250988365110 ) ) ;
#8921 = AXIS2_PLACEMENT_3D ( 'NONE', #1871, #15357, #5675 ) ;
#8922 = ORIENTED_EDGE ( 'NONE', *, *, #11197, .F. ) ;
#8923 = EDGE_CURVE ( 'NONE', #908, #3554, #14457, .T. ) ;
#8924 = VECTOR ( 'NONE', #7096, 1000.000000000000000 ) ;
#8925 = CARTESIAN_POINT ( 'NONE',  ( 0.02351960456806058766, 2.112255972321535502, -1.841465337348300535 ) ) ;
#8926 = DIRECTION ( 'NONE',  ( 0.000000000000000000, 0.000000000000000000, -1.000000000000000000 ) ) ;
#8927 = CARTESIAN_POINT ( 'NONE',  ( 0.000000000000000000, 7.511572993685799101E-16, -2.750000000000000444 ) ) ;
#8928 = CARTESIAN_POINT ( 'NONE',  ( -222.3946175954399678, 148.7843453045948650, -2.994737442266849570 ) ) ;
#8929 = VERTEX_POINT ( 'NONE', #12021 ) ;
#8930 = AXIS2_PLACEMENT_3D ( 'NONE', #5442, #675, #440 ) ;
#8931 = CARTESIAN_POINT ( 'NONE',  ( -217.4665255590759614, 153.5614479664741054, 7.035142701686511124 ) ) ;
#8932 = ORIENTED_EDGE ( 'NONE', *, *, #8276, .T. ) ;
#8933 = CARTESIAN_POINT ( 'NONE',  ( -171.5341366638640466, 120.9023397841524883, -5.092521039015617923 ) ) ;
#8934 = PLANE ( 'NONE',  #6098 ) ;
#8936 = ORIENTED_EDGE ( 'NONE', *, *, #2694, .F. ) ;
#8935 = CIRCLE ( 'NONE', #4127, 1.000000000000000888 ) ;
#8937 = PLANE ( 'NONE',  #12959 ) ;
#8938 = CARTESIAN_POINT ( 'NONE',  ( -64.00000000000002842, -179.8058001507315566, 84.88378295107887084 ) ) ;
#8939 = EDGE_CURVE ( 'NONE', #14692, #1447, #10096, .T. ) ;
#8940 = FACE_OUTER_BOUND ( 'NONE', #6105, .T. ) ;
#8941 = ORIENTED_EDGE ( 'NONE', *, *, #10592, .T. ) ;
#8942 = VECTOR ( 'NONE', #10891, 1000.000000000000000 ) ;
#8943 = ADVANCED_FACE ( 'NONE', ( #4844 ), #5787, .T. ) ;
#8944 = PRODUCT_DEFINITION ( 'UNKNOWN', '', #6275, #3941 ) ;
#8945 = ORIENTED_EDGE ( 'NONE', *, *, #13409, .T. ) ;
#8946 = AXIS2_PLACEMENT_3D ( 'NONE', #14982, #7678, #5532 ) ;
#8947 = EDGE_CURVE ( 'NONE', #815, #12968, #7336, .T. ) ;
#8948 = CARTESIAN_POINT ( 'NONE',  ( 51.39999999999999858, 0.000000000000000000, 0.000000000000000000 ) ) ;
#8949 = VERTEX_POINT ( 'NONE', #883 ) ;
#8950 = CARTESIAN_POINT ( 'NONE',  ( 190.0000000000000568, -179.3058001507315566, -51.45141194869120227 ) ) ;
#8951 = CARTESIAN_POINT ( 'NONE',  ( 190.0000000000000568, -178.8058001507315566, -30.31842631998718574 ) ) ;
#8952 = EDGE_LOOP ( 'NONE', ( #13056, #7488, #1404, #4887 ) ) ;
#8953 = ORIENTED_EDGE ( 'NONE', *, *, #10886, .F. ) ;
#8954 = CARTESIAN_POINT ( 'NONE',  ( -64.00000000000002842, -178.8058001507315566, -30.31842631998718574 ) ) ;
#8955 = CARTESIAN_POINT ( 'NONE',  ( 0.2456200930618629430, 3.175426480542944407, 1.454290997841272695E-16 ) ) ;
#8956 = CIRCLE ( 'NONE', #2128, 0.5000000000000001110 ) ;
#8957 = ORIENTED_EDGE ( 'NONE', *, *, #15518, .T. ) ;
#8958 = CARTESIAN_POINT ( 'NONE',  ( 208.8186272397570349, 39.68461847005694665, -7.558035125831273682 ) ) ;
#8959 = CARTESIAN_POINT ( 'NONE',  ( -34.79899788034579444, 48.72489408690345414, 9.975000000000001421 ) ) ;
#8960 = CARTESIAN_POINT ( 'NONE',  ( 6.399999999999999467, 0.000000000000000000, 0.000000000000000000 ) ) ;
#8961 = LINE ( 'NONE', #11397, #12739 ) ;
#8962 = DIRECTION ( 'NONE',  ( 1.000000000000000000, 1.669238443041287922E-16, 0.000000000000000000 ) ) ;
#8963 = EDGE_CURVE ( 'NONE', #6255, #8424, #1048, .T. ) ;
#8964 = EDGE_CURVE ( 'NONE', #10355, #9645, #8413, .T. ) ;
#8965 = VECTOR ( 'NONE', #4938, 1000.000000000000000 ) ;
#8966 = DIRECTION ( 'NONE',  ( -0.000000000000000000, 1.000000000000000000, 0.000000000000000000 ) ) ;
#8967 = ORIENTED_EDGE ( 'NONE', *, *, #9496, .T. ) ;
#8968 = DIRECTION ( 'NONE',  ( 1.000000000000000000, 0.000000000000000000, 0.000000000000000000 ) ) ;
#8969 = CARTESIAN_POINT ( 'NONE',  ( 114.0000000000000568, 64.53993994372673626, 15.00000000000035172 ) ) ;
#8970 = CARTESIAN_POINT ( 'NONE',  ( -170.0916760340589349, 128.4977246429275226, -0.4609024664951656969 ) ) ;
#8971 = FACE_OUTER_BOUND ( 'NONE', #201, .T. ) ;
#8972 = VERTEX_POINT ( 'NONE', #10613 ) ;
#8973 = CARTESIAN_POINT ( 'NONE',  ( -181.9060177919747048, 118.7341819232202909, 5.367833425961690885 ) ) ;
#8974 = CARTESIAN_POINT ( 'NONE',  ( 191.4070815280707052, 39.69144961696751039, -1.360995051912267106 ) ) ;
#8975 = ORIENTED_EDGE ( 'NONE', *, *, #3132, .F. ) ;
#8976 = EDGE_CURVE ( 'NONE', #12405, #15483, #4603, .T. ) ;
#8977 = TOROIDAL_SURFACE ( 'NONE', #373, 5.400000000000000355, 0.4000000000000000222 ) ;
#8978 = CARTESIAN_POINT ( 'NONE',  ( 191.4922098844999425, 60.63967129342340456, 5.000000000000000000 ) ) ;
#8979 = DIRECTION ( 'NONE',  ( 1.000000000000000000, 0.000000000000000000, 0.000000000000000000 ) ) ;
#8980 = VECTOR ( 'NONE', #3738, 1000.000000000000000 ) ;
#8981 = CARTESIAN_POINT ( 'NONE',  ( 200.1062858801516597, 40.86394065090267702, 12.00000000000001066 ) ) ;
#8982 = FACE_BOUND ( 'NONE', #6013, .T. ) ;
#8983 = ORIENTED_EDGE ( 'NONE', *, *, #4111, .T. ) ;
#8984 = DIRECTION ( 'NONE',  ( -1.000000000000000000, 0.000000000000000000, 0.000000000000000000 ) ) ;
#8985 = AXIS2_PLACEMENT_3D ( 'NONE', #8053, #838, #9306 ) ;
#8986 = DIRECTION ( 'NONE',  ( -0.8731965799097685110, 0.4873681696970817434, 0.000000000000000000 ) ) ;
#8987 = DIRECTION ( 'NONE',  ( 1.000000000000000000, -0.000000000000000000, -0.000000000000000000 ) ) ;
#8988 = ORIENTED_EDGE ( 'NONE', *, *, #2766, .T. ) ;
#8989 = AXIS2_PLACEMENT_3D ( 'NONE', #1521, #14774, #13513 ) ;
#8990 = CARTESIAN_POINT ( 'NONE',  ( -64.00000000000002842, -178.9449732516916072, 64.32815825124539799 ) ) ;
#8991 = ORIENTED_EDGE ( 'NONE', *, *, #7310, .F. ) ;
#8992 = ADVANCED_FACE ( 'NONE', ( #13189 ), #1190, .F. ) ;
#8993 = ORIENTED_EDGE ( 'NONE', *, *, #11447, .T. ) ;
#8994 = CARTESIAN_POINT ( 'NONE',  ( -110.0000000000000426, 19.53993994372674337, 24.99999999999999645 ) ) ;
#8995 = LINE ( 'NONE', #432, #1339 ) ;
#8996 = DIRECTION ( 'NONE',  ( 0.8731965799097682890, -0.4873681696970819099, 0.000000000000000000 ) ) ;
#8997 = FACE_OUTER_BOUND ( 'NONE', #5763, .T. ) ;
#8998 = CARTESIAN_POINT ( 'NONE',  ( -163.7578731888787331, 108.1608566195349113, 2.431557144026070372 ) ) ;
#8999 = AXIS2_PLACEMENT_3D ( 'NONE', #6747, #560, #11480 ) ;
#9000 = AXIS2_PLACEMENT_3D ( 'NONE', #15588, #11982, #14329 ) ;
#9001 = DIRECTION ( 'NONE',  ( 0.000000000000000000, 1.000000000000000000, 6.938893903907227145E-17 ) ) ;
#9002 = DIRECTION ( 'NONE',  ( -0.000000000000000000, 1.000000000000000000, -0.000000000000000000 ) ) ;
#9003 = LINE ( 'NONE', #9879, #4071 ) ;
#9004 = CARTESIAN_POINT ( 'NONE',  ( -173.4445345933175986, 43.15250799526725700, 0.000000000000000000 ) ) ;
#9005 = ORIENTED_EDGE ( 'NONE', *, *, #4922, .T. ) ;
#9006 = CARTESIAN_POINT ( 'NONE',  ( -218.4940076538873939, 155.7729003073443437, 3.755297502929312969 ) ) ;
#9007 = EDGE_LOOP ( 'NONE', ( #7031, #4038, #6287, #1891 ) ) ;
#9008 = CARTESIAN_POINT ( 'NONE',  ( 0.4969600502617610993, -8.860760056385762695, -0.6527133886630168691 ) ) ;
#9009 = AXIS2_PLACEMENT_3D ( 'NONE', #14808, #3934, #1475 ) ;
#9010 = DIRECTION ( 'NONE',  ( 0.000000000000000000, -0.000000000000000000, -1.000000000000000000 ) ) ;
#9011 = ORIENTED_EDGE ( 'NONE', *, *, #4093, .F. ) ;
#9012 = CARTESIAN_POINT ( 'NONE',  ( -76.50000000000002842, -178.8058001507315566, 53.19066787724494816 ) ) ;
#9013 = DIRECTION ( 'NONE',  ( -1.000000000000000000, 0.000000000000000000, 0.000000000000000000 ) ) ;
#9014 = CARTESIAN_POINT ( 'NONE',  ( 0.000000000000000000, 19.53993994372674337, 2.905405074819403421E-15 ) ) ;
#9016 = ORIENTED_EDGE ( 'NONE', *, *, #989, .T. ) ;
#9015 = EDGE_CURVE ( 'NONE', #12471, #6255, #12109, .T. ) ;
#9017 = APPLICATION_PROTOCOL_DEFINITION ( 'draft international standard', 'automotive_design', 1998, #2417 ) ;
#9018 = AXIS2_PLACEMENT_3D ( 'NONE', #4157, #8996, #13789 ) ;
#9019 = ORIENTED_EDGE ( 'NONE', *, *, #11245, .T. ) ;
#9020 = CARTESIAN_POINT ( 'NONE',  ( 202.4110361843541455, 29.59410989755560806, -6.585651355106874050 ) ) ;
#9021 = CYLINDRICAL_SURFACE ( 'NONE', #169, 1.000000000000000888 ) ;
#9022 = ORIENTED_EDGE ( 'NONE', *, *, #7503, .T. ) ;
#9023 = CARTESIAN_POINT ( 'NONE',  ( 21.71949999999999648, 0.000000000000000000, 0.000000000000000000 ) ) ;
#9024 = CARTESIAN_POINT ( 'NONE',  ( 124.2806775638430281, 45.00321902537314145, 7.600000000000002309 ) ) ;
#9025 = ORIENTED_EDGE ( 'NONE', *, *, #6930, .F. ) ;
#9026 = ORIENTED_EDGE ( 'NONE', *, *, #5574, .T. ) ;
#9027 = DIRECTION ( 'NONE',  ( -0.000000000000000000, -0.000000000000000000, -1.000000000000000000 ) ) ;
#9028 = LINE ( 'NONE', #6742, #11885 ) ;
#9029 = EDGE_CURVE ( 'NONE', #10578, #8562, #3346, .T. ) ;
#9030 = VERTEX_POINT ( 'NONE', #9426 ) ;
#9031 = CARTESIAN_POINT ( 'NONE',  ( 201.2541767070109984, 32.14103196098812987, -5.186035738131804962 ) ) ;
#9032 = CARTESIAN_POINT ( 'NONE',  ( 170.6368569633305583, 57.90162049975850067, -0.9107274384406883749 ) ) ;
#9033 = AXIS2_PLACEMENT_3D ( 'NONE', #15440, #13153, #3095 ) ;
#9034 = CARTESIAN_POINT ( 'NONE',  ( 178.0000000000000853, -179.8058001507315566, 65.31842631998698323 ) ) ;
#9035 = DIRECTION ( 'NONE',  ( 1.000000000000000000, 0.000000000000000000, -0.000000000000000000 ) ) ;
#9036 = PRODUCT_DEFINITION_SHAPE ( 'NONE', 'NONE',  #15633 ) ;
#9037 = VECTOR ( 'NONE', #4083, 1000.000000000000000 ) ;
#9038 = CARTESIAN_POINT ( 'NONE',  ( 5.799999999999999822, 9.237604307034018802, 0.000000000000000000 ) ) ;
#9039 = VERTEX_POINT ( 'NONE', #2153 ) ;
#9040 = DIRECTION ( 'NONE',  ( 0.000000000000000000, -1.000000000000000000, 0.000000000000000000 ) ) ;
#9041 = AXIS2_PLACEMENT_3D ( 'NONE', #3203, #743, #6769 ) ;
#9042 = CARTESIAN_POINT ( 'NONE',  ( -179.6520503532206021, 128.8169225571170102, -4.640918829492417075 ) ) ;
#9043 = FACE_OUTER_BOUND ( 'NONE', #6090, .T. ) ;
#9044 = ORIENTED_EDGE ( 'NONE', *, *, #12063, .T. ) ;
#9045 = CARTESIAN_POINT ( 'NONE',  ( -184.9748306402843809, 119.2867206268225999, 3.478895870929497036 ) ) ;
#9046 = CARTESIAN_POINT ( 'NONE',  ( 209.5385712735872517, 33.62447922832576097, -6.247773722084159154 ) ) ;
#9047 = ORIENTED_EDGE ( 'NONE', *, *, #7528, .T. ) ;
#9048 = EDGE_CURVE ( 'NONE', #14876, #9030, #5819, .T. ) ;
#9050 = EDGE_CURVE ( 'NONE', #12061, #6010, #6263, .T. ) ;
#9049 = EDGE_CURVE ( 'NONE', #9280, #5867, #13031, .T. ) ;
#9051 = CIRCLE ( 'NONE', #14321, 0.5000000000000001110 ) ;
#9052 = LINE ( 'NONE', #14867, #12697 ) ;
#9053 = DIRECTION ( 'NONE',  ( 0.9296197478520974444, 0.3660421972118351741, -0.04266420354037655377 ) ) ;
#9054 =( GEOMETRIC_REPRESENTATION_CONTEXT ( 3 ) GLOBAL_UNCERTAINTY_ASSIGNED_CONTEXT ( ( #11362 ) ) GLOBAL_UNIT_ASSIGNED_CONTEXT ( ( #1061, #13937, #10701 ) ) REPRESENTATION_CONTEXT ( 'NONE', 'WORKASPACE' ) );
#9055 = DIRECTION ( 'NONE',  ( -1.000000000000000000, -2.751328491981765035E-32, 3.965082230804130220E-16 ) ) ;
#9056 = PLANE ( 'NONE',  #11661 ) ;
#9057 = ORIENTED_EDGE ( 'NONE', *, *, #10464, .T. ) ;
#9058 = CARTESIAN_POINT ( 'NONE',  ( 184.0000000000000568, 17.53993994372673626, 47.49999999999997868 ) ) ;
#9059 = CARTESIAN_POINT ( 'NONE',  ( -177.2599095556795419, 121.3508012008377932, 9.485662293947264345 ) ) ;
#9060 = DIRECTION ( 'NONE',  ( -9.657073818396194363E-16, -0.9902680687415711391, 0.1391731009600592484 ) ) ;
#9061 = CIRCLE ( 'NONE', #15087, 1.499999999999994227 ) ;
#9062 = CYLINDRICAL_SURFACE ( 'NONE', #4523, 1.000000000000000888 ) ;
#9063 = ORIENTED_EDGE ( 'NONE', *, *, #10011, .T. ) ;
#9064 = AXIS2_PLACEMENT_3D ( 'NONE', #6920, #971, #3123 ) ;
#9065 = DIRECTION ( 'NONE',  ( -1.000000000000000000, 0.000000000000000000, 0.000000000000000000 ) ) ;
#9066 = AXIS2_PLACEMENT_3D ( 'NONE', #10526, #1124, #2233 ) ;
#9067 = EDGE_LOOP ( 'NONE', ( #9151, #4759, #1278, #450 ) ) ;
#9068 = ORIENTED_EDGE ( 'NONE', *, *, #5870, .F. ) ;
#9069 = CARTESIAN_POINT ( 'NONE',  ( -151.1638989062950031, 108.2516363225298619, 9.821053999514628430 ) ) ;
#9070 = CARTESIAN_POINT ( 'NONE',  ( -61.94838851346079167, -179.3058001507315566, 84.88378295107887084 ) ) ;
#9071 = FACE_OUTER_BOUND ( 'NONE', #5300, .T. ) ;
#9072 = CARTESIAN_POINT ( 'NONE',  ( -171.3372721184446164, 121.2550535197920851, 9.804730088504793883 ) ) ;
#9073 = DIRECTION ( 'NONE',  ( 0.000000000000000000, 0.000000000000000000, -1.000000000000000000 ) ) ;
#9074 = AXIS2_PLACEMENT_3D ( 'NONE', #9827, #3737, #13361 ) ;
#9075 = DIRECTION ( 'NONE',  ( 3.965082230804130220E-16, -0.000000000000000000, -1.000000000000000000 ) ) ;
#9076 = CIRCLE ( 'NONE', #6296, 1.500000000000001332 ) ;
#9077 = AXIS2_PLACEMENT_3D ( 'NONE', #1900, #2136, #4503 ) ;
#9078 = CARTESIAN_POINT ( 'NONE',  ( -64.00000000000002842, 15.53993994372673804, 38.07518420361041933 ) ) ;
#9079 = DIRECTION ( 'NONE',  ( 0.000000000000000000, -1.000000000000000000, -6.938893903907222067E-15 ) ) ;
#9080 = EDGE_CURVE ( 'NONE', #14978, #13487, #10612, .T. ) ;
#9081 = FACE_BOUND ( 'NONE', #1388, .T. ) ;
#9082 = VECTOR ( 'NONE', #11270, 1000.000000000000000 ) ;
#9083 = DIRECTION ( 'NONE',  ( 0.000000000000000000, 0.000000000000000000, -1.000000000000000000 ) ) ;
#9084 = EDGE_LOOP ( 'NONE', ( #10792, #13275, #10047, #10111 ) ) ;
#9085 = AXIS2_PLACEMENT_3D ( 'NONE', #10847, #14067, #3262 ) ;
#9086 = AXIS2_PLACEMENT_3D ( 'NONE', #5998, #7861, #4356 ) ;
#9087 = ORIENTED_EDGE ( 'NONE', *, *, #13676, .F. ) ;
#9088 = CARTESIAN_POINT ( 'NONE',  ( 0.000000000000000000, 15.53993994372673981, 7.305634244248866343E-16 ) ) ;
#9089 = DIRECTION ( 'NONE',  ( -0.000000000000000000, 1.000000000000000000, 0.000000000000000000 ) ) ;
#9090 = CIRCLE ( 'NONE', #3034, 0.5000000000000001110 ) ;
#9091 = ORIENTED_EDGE ( 'NONE', *, *, #6638, .T. ) ;
#9092 = PLANE ( 'NONE',  #11208 ) ;
#9093 = DIRECTION ( 'NONE',  ( 1.000000000000000000, -0.000000000000000000, -0.000000000000000000 ) ) ;
#9094 = CIRCLE ( 'NONE', #12600, 0.5000000000000001110 ) ;
#9095 = CYLINDRICAL_SURFACE ( 'NONE', #9922, 0.5000000000000004441 ) ;
#9096 = ORIENTED_EDGE ( 'NONE', *, *, #15476, .T. ) ;
#9097 = AXIS2_PLACEMENT_3D ( 'NONE', #3296, #14096, #5816 ) ;
#9098 = EDGE_CURVE ( 'NONE', #5229, #3979, #4042, .T. ) ;
#9099 = APPLICATION_PROTOCOL_DEFINITION ( 'draft international standard', 'automotive_design', 1998, #8885 ) ;
#9100 = ORIENTED_EDGE ( 'NONE', *, *, #15100, .T. ) ;
#9101 = CARTESIAN_POINT ( 'NONE',  ( 198.3593989614203963, 52.60648038231462920, -8.258707374242266752 ) ) ;
#9102 = LINE ( 'NONE', #11833, #14805 ) ;
#9103 = VERTEX_POINT ( 'NONE', #11776 ) ;
#9104 = DIRECTION ( 'NONE',  ( -0.000000000000000000, -0.000000000000000000, -1.000000000000000000 ) ) ;
#9105 = CARTESIAN_POINT ( 'NONE',  ( 114.0000000000000568, 64.53993994372673626, 15.00000000000035172 ) ) ;
#9106 = ORIENTED_EDGE ( 'NONE', *, *, #5572, .F. ) ;
#9107 = ORIENTED_EDGE ( 'NONE', *, *, #6839, .T. ) ;
#9108 = CARTESIAN_POINT ( 'NONE',  ( 184.0000000000000568, 15.53993994372673626, 47.49999999999997868 ) ) ;
#9109 = EDGE_CURVE ( 'NONE', #1434, #1700, #9614, .T. ) ;
#9110 = CARTESIAN_POINT ( 'NONE',  ( 0.000000000000000000, 17.53993994372673981, 2.674108611355829274E-15 ) ) ;
#9111 = AXIS2_PLACEMENT_3D ( 'NONE', #6627, #7811, #1632 ) ;
#9112 = EDGE_LOOP ( 'NONE', ( #1376, #6772, #1279, #14947 ) ) ;
#9113 = CARTESIAN_POINT ( 'NONE',  ( 203.0658429208174880, 48.83360436048501896, -0.9158339742359169477 ) ) ;
#9114 = CARTESIAN_POINT ( 'NONE',  ( 71.96535645333923981, 38.79159067395544014, 10.00000000000000178 ) ) ;
#9115 = DIRECTION ( 'NONE',  ( -1.000000000000000000, 0.000000000000000000, 0.000000000000000000 ) ) ;
#9116 = CARTESIAN_POINT ( 'NONE',  ( -70.00000000000000000, -201.3058001507315566, 76.45141194869098911 ) ) ;
#9117 = DIRECTION ( 'NONE',  ( 1.000000000000000000, -0.000000000000000000, -0.000000000000000000 ) ) ;
#9118 = VECTOR ( 'NONE', #8245, 1000.000000000000000 ) ;
#9119 = EDGE_CURVE ( 'NONE', #5590, #6168, #10670, .T. ) ;
#9120 = DIRECTION ( 'NONE',  ( 0.000000000000000000, 0.000000000000000000, 1.000000000000000000 ) ) ;
#9121 = TOROIDAL_SURFACE ( 'NONE', #9378, 1.000000000000000000, 0.5000000000000000000 ) ;
#9122 = ORIENTED_EDGE ( 'NONE', *, *, #2967, .F. ) ;
#9123 = CARTESIAN_POINT ( 'NONE',  ( 190.0000000000000568, 15.53993994372673981, -3.075184203610571654 ) ) ;
#9124 = CARTESIAN_POINT ( 'NONE',  ( -178.3861577417919477, 131.0834419243807076, -2.963320117457100888 ) ) ;
#9125 = CARTESIAN_POINT ( 'NONE',  ( 190.0000000000001137, -178.8058001507315566, 65.31842631998698323 ) ) ;
#9126 = ORIENTED_EDGE ( 'NONE', *, *, #12504, .F. ) ;
#9127 = CARTESIAN_POINT ( 'NONE',  ( -173.7777028115792177, 116.1670890754947152, -0.7095712321138001322 ) ) ;
#9128 = UNCERTAINTY_MEASURE_WITH_UNIT (LENGTH_MEASURE( 1.000000000000000082E-05 ), #13081, 'distance_accuracy_value', 'NONE');
#9129 = CARTESIAN_POINT ( 'NONE',  ( 211.8917419932436985, 39.20340779279173660, -5.995121456379560954 ) ) ;
#9130 = ORIENTED_EDGE ( 'NONE', *, *, #7416, .T. ) ;
#9131 = AXIS2_PLACEMENT_3D ( 'NONE', #4589, #8403, #13254 ) ;
#9132 = FACE_OUTER_BOUND ( 'NONE', #3055, .T. ) ;
#9133 = CARTESIAN_POINT ( 'NONE',  ( 190.5000000000000853, 17.53993994372673626, 52.49999999999997868 ) ) ;
#9134 = EDGE_CURVE ( 'NONE', #2673, #3949, #8522, .T. ) ;
#9135 = DIRECTION ( 'NONE',  ( 0.000000000000000000, 0.1391731009600592484, 0.9902680687415712502 ) ) ;
#9136 = SHAPE_REPRESENTATION_RELATIONSHIP ( 'NONE' , 'NONE' ,  #11876, #9237 ) ;
#9137 = CARTESIAN_POINT ( 'NONE',  ( 0.000000000000000000, 0.000000000000000000, 5.000000000000000000 ) ) ;
#9138 = ADVANCED_FACE ( 'NONE', ( #10594 ), #15463, .F. ) ;
#9139 = EDGE_CURVE ( 'NONE', #9639, #4933, #4652, .T. ) ;
#9140 = ORIENTED_EDGE ( 'NONE', *, *, #7180, .F. ) ;
#9141 = AXIS2_PLACEMENT_3D ( 'NONE', #7882, #12906, #6617 ) ;
#9142 = CARTESIAN_POINT ( 'NONE',  ( 17.41029453487719181, 40.04259805664093363, 7.600000000000002309 ) ) ;
#9143 = CARTESIAN_POINT ( 'NONE',  ( -209.3130641152695830, 145.0632059852189570, 9.578254705571840333 ) ) ;
#9144 = DIRECTION ( 'NONE',  ( 0.000000000000000000, 0.000000000000000000, 1.000000000000000000 ) ) ;
#9145 = ADVANCED_FACE ( 'NONE', ( #4658 ), #9487, .F. ) ;
#9146 = VECTOR ( 'NONE', #1318, 1000.000000000000000 ) ;
#9147 = CARTESIAN_POINT ( 'NONE',  ( -155.6734249082932422, 110.4587098853260585, -4.906289360893208773 ) ) ;
#9148 = ORIENTED_EDGE ( 'NONE', *, *, #10921, .T. ) ;
#9149 = FACE_OUTER_BOUND ( 'NONE', #1125, .T. ) ;
#9150 = VERTEX_POINT ( 'NONE', #12214 ) ;
#9151 = ORIENTED_EDGE ( 'NONE', *, *, #11407, .F. ) ;
#9152 = DIRECTION ( 'NONE',  ( 0.000000000000000000, 0.000000000000000000, -1.000000000000000000 ) ) ;
#9153 = DIRECTION ( 'NONE',  ( -0.000000000000000000, -0.000000000000000000, 1.000000000000000000 ) ) ;
#9154 = FACE_BOUND ( 'NONE', #12517, .T. ) ;
#9155 = DIRECTION ( 'NONE',  ( 1.000000000000000000, 0.000000000000000000, 0.000000000000000000 ) ) ;
#9156 = CARTESIAN_POINT ( 'NONE',  ( -217.6093082865582460, 153.3060710425520199, -2.530008684083509873 ) ) ;
#9157 = DIRECTION ( 'NONE',  ( -0.3297523322010256219, -0.9440639390088612082, 0.002584273796984222320 ) ) ;
#9158 = CLOSED_SHELL ( 'NONE', ( #7052, #11520, #11716, #4711, #11427, #7037, #8149, #120, #5085, #911, #13065, #7371, #11655, #1987, #4267, #2148, #2895, #9992, #11785, #12901, #6479, #13863, #5660, #2512, #13849, #12209, #3804, #15541, #418, #9482, #7605, #8074, #7978, #3550, #7128, #3645, #7703, #11947, #5029, #14259, #4110, #15355, #10455, #2950, #439, #6138, #13986, #6826 ) ) ;
#9159 = EDGE_CURVE ( 'NONE', #8585, #555, #11365, .T. ) ;
#9160 = ADVANCED_FACE ( 'NONE', ( #11038 ), #11703, .T. ) ;
#9161 = DIRECTION ( 'NONE',  ( -0.000000000000000000, -0.9902680687415702510, -0.1391731009600660485 ) ) ;
#9162 = UNCERTAINTY_MEASURE_WITH_UNIT (LENGTH_MEASURE( 1.000000000000000082E-05 ), #9211, 'distance_accuracy_value', 'NONE');
#9163 = DIRECTION ( 'NONE',  ( -0.000000000000000000, -1.000000000000000000, -0.000000000000000000 ) ) ;
#9164 = CARTESIAN_POINT ( 'NONE',  ( 224.0000000000000853, 59.53993994372674337, 10.00000000000000178 ) ) ;
#9165 = CARTESIAN_POINT ( 'NONE',  ( -222.5645123348136281, 148.4799522100312572, -2.927675643254317173 ) ) ;
#9166 = EDGE_LOOP ( 'NONE', ( #3993, #7363 ) ) ;
#9167 = VERTEX_POINT ( 'NONE', #3327 ) ;
#9168 = LINE ( 'NONE', #14038, #5772 ) ;
#9169 = VECTOR ( 'NONE', #8915, 1000.000000000000000 ) ;
#9170 = FACE_OUTER_BOUND ( 'NONE', #332, .T. ) ;
#9171 = DIRECTION ( 'NONE',  ( 1.000000000000000000, 0.000000000000000000, 0.000000000000000000 ) ) ;
#9172 = CARTESIAN_POINT ( 'NONE',  ( 168.4217645774054120, 62.57671370024034729, -0.9107274384406881529 ) ) ;
#9173 = CARTESIAN_POINT ( 'NONE',  ( -34.29999999999994742, 62.13993994372673768, 15.00000000000139977 ) ) ;
#9174 = PRODUCT ( 'Lower Fixed Bed Shear Blade', 'Lower Fixed Bed Shear Blade', '', ( #12548 ) ) ;
#9175 = EDGE_CURVE ( 'NONE', #828, #3731, #8166, .T. ) ;
#9176 = DIRECTION ( 'NONE',  ( 1.000000000000000000, 0.000000000000000000, 0.000000000000000000 ) ) ;
#9177 = ORIENTED_EDGE ( 'NONE', *, *, #7073, .T. ) ;
#9178 = CONTEXT_DEPENDENT_SHAPE_REPRESENTATION ( #4840, #1961 ) ;
#9179 = ORIENTED_EDGE ( 'NONE', *, *, #15518, .F. ) ;
#9180 = CARTESIAN_POINT ( 'NONE',  ( 192.8417602520171670, 50.27412068648693122, -8.008884321912063342 ) ) ;
#9181 = ORIENTED_EDGE ( 'NONE', *, *, #1505, .T. ) ;
#9182 = CARTESIAN_POINT ( 'NONE',  ( -173.4445345933175986, 43.15250799526725700, 5.000000000000000000 ) ) ;
#9183 = VECTOR ( 'NONE', #9768, 1000.000000000000000 ) ;
#9184 = CARTESIAN_POINT ( 'NONE',  ( -225.7021444021470415, 142.8583918362506608, 2.570299564593518937 ) ) ;
#9185 = EDGE_LOOP ( 'NONE', ( #3236, #6647, #12499, #4229 ) ) ;
#9186 = VERTEX_POINT ( 'NONE', #13783 ) ;
#9187 = CARTESIAN_POINT ( 'NONE',  ( 171.7208925888976978, 62.57671370024034729, -0.9107274384406883749 ) ) ;
#9188 = ORIENTED_EDGE ( 'NONE', *, *, #9984, .F. ) ;
#9189 = CARTESIAN_POINT ( 'NONE',  ( 194.7957337413261030, 33.86335648926068842, -5.558215102112974648 ) ) ;
#9190 = DIRECTION ( 'NONE',  ( 1.000000000000000000, -2.751328491981765035E-32, 3.965082230804130220E-16 ) ) ;
#9191 = EDGE_CURVE ( 'NONE', #12014, #6280, #15377, .T. ) ;
#9192 = VECTOR ( 'NONE', #9232, 1000.000000000000114 ) ;
#9193 = DIRECTION ( 'NONE',  ( 0.000000000000000000, 0.8660254037844375974, -0.5000000000000019984 ) ) ;
#9194 = DIRECTION ( 'NONE',  ( -0.000000000000000000, -0.000000000000000000, -1.000000000000000000 ) ) ;
#9195 = DIRECTION ( 'NONE',  ( 0.000000000000000000, 0.000000000000000000, 1.000000000000000000 ) ) ;
#9196 = CIRCLE ( 'NONE', #14464, 2.000000000000001776 ) ;
#9197 = CYLINDRICAL_SURFACE ( 'NONE', #10585, 0.5000000000000004441 ) ;
#9198 = VERTEX_POINT ( 'NONE', #11122 ) ;
#9199 = CARTESIAN_POINT ( 'NONE',  ( -85.99999999999994316, 56.53993994372675047, 15.00000000000174794 ) ) ;
#9200 = VECTOR ( 'NONE', #3381, 1000.000000000000000 ) ;
#9201 = CARTESIAN_POINT ( 'NONE',  ( -188.0666105031049824, 138.5497687542270739, -0.4547266291960739282 ) ) ;
#9202 = DIRECTION ( 'NONE',  ( -0.000000000000000000, 1.000000000000000000, 6.938893903907227145E-17 ) ) ;
#9203 = VERTEX_POINT ( 'NONE', #10090 ) ;
#9204 = CARTESIAN_POINT ( 'NONE',  ( -178.4226240946890130, 124.9752285324798606, -5.265047855996060733 ) ) ;
#9205 = CARTESIAN_POINT ( 'NONE',  ( 192.8417602520171670, 50.27412068648693122, -8.008884321912063342 ) ) ;
#9206 = ORIENTED_EDGE ( 'NONE', *, *, #12044, .F. ) ;
#9207 = DIRECTION ( 'NONE',  ( 0.9296197478520975555, 0.3660421972118350631, -0.04266420354037653295 ) ) ;
#9208 = LINE ( 'NONE', #15027, #377 ) ;
#9209 = EDGE_CURVE ( 'NONE', #10379, #15150, #8105, .T. ) ;
#9210 = ORIENTED_EDGE ( 'NONE', *, *, #4674, .T. ) ;
#9211 =( LENGTH_UNIT ( ) NAMED_UNIT ( * ) SI_UNIT ( .MILLI., .METRE. ) );
#9212 = DIRECTION ( 'NONE',  ( 0.000000000000000000, 6.938893903907227145E-17, -1.000000000000000000 ) ) ;
#9213 = ORIENTED_EDGE ( 'NONE', *, *, #8471, .F. ) ;
#9214 = CARTESIAN_POINT ( 'NONE',  ( 178.0000000000000853, 23.05038067821381986, -0.9395626039331514967 ) ) ;
#9215 = CARTESIAN_POINT ( 'NONE',  ( -200.1466204956978459, 130.0968966444285968, 7.918248976830634334 ) ) ;
#9216 = CYLINDRICAL_SURFACE ( 'NONE', #4494, 1.699999999999996625 ) ;
#9217 = CARTESIAN_POINT ( 'NONE',  ( 0.08224679563971239171, 7.710515798486361483, 2.644994884459111795 ) ) ;
#9218 = ORIENTED_EDGE ( 'NONE', *, *, #3919, .F. ) ;
#9219 = CARTESIAN_POINT ( 'NONE',  ( 164.0000000000000568, 56.53993994372675047, 16.70000000000000995 ) ) ;
#9220 = AXIS2_PLACEMENT_3D ( 'NONE', #9447, #12981, #7319 ) ;
#9221 = EDGE_LOOP ( 'NONE', ( #14671, #10672 ) ) ;
#9222 = ORIENTED_EDGE ( 'NONE', *, *, #6089, .T. ) ;
#9223 = CARTESIAN_POINT ( 'NONE',  ( -152.4086188282879277, 107.2728346664360259, 9.411501811869209533 ) ) ;
#9224 = CARTESIAN_POINT ( 'NONE',  ( 190.5000000000000568, 19.53993994372674692, -17.50000000000002487 ) ) ;
#9225 = EDGE_CURVE ( 'NONE', #11731, #8472, #13625, .T. ) ;
#9226 = FACE_BOUND ( 'NONE', #748, .T. ) ;
#9227 = CARTESIAN_POINT ( 'NONE',  ( -168.1084462739055425, 127.0400018604442636, 5.672933193154669596 ) ) ;
#9228 = CARTESIAN_POINT ( 'NONE',  ( -224.3995683171452242, 145.1921613625067096, -3.326444132835047807 ) ) ;
#9229 = DIRECTION ( 'NONE',  ( 0.000000000000000000, 0.000000000000000000, -1.000000000000000000 ) ) ;
#9230 = CIRCLE ( 'NONE', #14998, 3.500000000000003109 ) ;
#9231 = FACE_OUTER_BOUND ( 'NONE', #14468, .T. ) ;
#9232 = DIRECTION ( 'NONE',  ( -0.7071067811865500152, 8.659560562354904508E-17, -0.7071067811865451302 ) ) ;
#9233 = DIRECTION ( 'NONE',  ( 0.000000000000000000, 0.000000000000000000, -1.000000000000000000 ) ) ;
#9234 = LINE ( 'NONE', #6949, #238 ) ;
#9235 = CARTESIAN_POINT ( 'NONE',  ( -219.8602732323815587, 153.3250210559709217, -0.6604898276721635764 ) ) ;
#9236 = EDGE_LOOP ( 'NONE', ( #6025, #9206 ) ) ;
#9237 = ADVANCED_BREP_SHAPE_REPRESENTATION ( '', ( #10736, #12337 ), #5251 ) ;
#9238 = DIRECTION ( 'NONE',  ( 1.000000000000000000, 0.000000000000000000, 0.000000000000000000 ) ) ;
#9239 = VERTEX_POINT ( 'NONE', #4079 ) ;
#9240 = CARTESIAN_POINT ( 'NONE',  ( -174.2824251065520968, 115.9783496305641535, 2.177446462082195389 ) ) ;
#9241 = LINE ( 'NONE', #13803, #4575 ) ;
#9242 = ADVANCED_FACE ( 'NONE', ( #2981, #11196, #425 ), #7570, .F. ) ;
#9243 = EDGE_CURVE ( 'NONE', #158, #15257, #507, .T. ) ;
#9244 = ORIENTED_EDGE ( 'NONE', *, *, #2331, .F. ) ;
#9245 = EDGE_CURVE ( 'NONE', #15197, #6193, #1777, .T. ) ;
#9246 = LINE ( 'NONE', #13973, #8859 ) ;
#9247 = CIRCLE ( 'NONE', #904, 0.5000000000000004441 ) ;
#9248 = VECTOR ( 'NONE', #14177, 1000.000000000000000 ) ;
#9249 = DIRECTION ( 'NONE',  ( 0.000000000000000000, 0.000000000000000000, -1.000000000000000000 ) ) ;
#9250 = VERTEX_POINT ( 'NONE', #12443 ) ;
#9251 = B_SPLINE_CURVE_WITH_KNOTS ( 'NONE', 3,
 ( #2761, #4011, #8925, #2921, #8842, #522 ),
 .UNSPECIFIED., .F., .F.,
 ( 4, 2, 4 ),
 ( 0.001606744326298692937, 0.002406996759593252235, 0.003207249192887811316 ),
 .UNSPECIFIED. ) ;
#9252 = CONTEXT_DEPENDENT_SHAPE_REPRESENTATION ( #13492, #15315 ) ;
#9253 = EDGE_LOOP ( 'NONE', ( #6730, #4306 ) ) ;
#9254 = CARTESIAN_POINT ( 'NONE',  ( 204.1803465669382547, 51.62486026858844212, 0.6453845751958426913 ) ) ;
#9255 = FACE_OUTER_BOUND ( 'NONE', #14123, .T. ) ;
#9256 = ORIENTED_EDGE ( 'NONE', *, *, #2314, .T. ) ;
#9257 = VECTOR ( 'NONE', #12376, 1000.000000000000000 ) ;
#9258 = DIRECTION ( 'NONE',  ( -0.7071067811865474617, 8.659560562354932858E-17, 0.7071067811865474617 ) ) ;
#9259 = ADVANCED_FACE ( 'NONE', ( #7732 ), #2672, .T. ) ;
#9260 = CARTESIAN_POINT ( 'NONE',  ( -61.94838851346079167, -179.3058001507315566, -29.88378295107906624 ) ) ;
#9261 = VERTEX_POINT ( 'NONE', #5114 ) ;
#9262 = VERTEX_POINT ( 'NONE', #276 ) ;
#9263 = LINE ( 'NONE', #6896, #4743 ) ;
#9264 = CARTESIAN_POINT ( 'NONE',  ( -70.00000000000000000, 15.53993994372673981, -10.99999999999999645 ) ) ;
#9265 = EDGE_LOOP ( 'NONE', ( #8558, #15248, #9213, #7440 ) ) ;
#9266 = CARTESIAN_POINT ( 'NONE',  ( -70.00000000000000000, -179.3058001507315566, 74.95141194869098911 ) ) ;
#9267 = DIRECTION ( 'NONE',  ( 1.000000000000000000, 0.000000000000000000, 0.000000000000000000 ) ) ;
#9268 = FACE_OUTER_BOUND ( 'NONE', #3594, .T. ) ;
#9269 = FACE_OUTER_BOUND ( 'NONE', #9, .T. ) ;
#9270 = B_SPLINE_CURVE_WITH_KNOTS ( 'NONE', 3,
 ( #12595, #14957, #13703, #7649, #7889, #12441, #744, #4148, #1630, #1784, #6624, #588, #15034, #663, #4305, #9147, #2906, #5502 ),
 .UNSPECIFIED., .F., .F.,
 ( 4, 2, 2, 2, 2, 2, 2, 2, 4 ),
 ( 1.482148387583608474E-17, 0.0003981710496980508571, 0.0007963420993960869691, 0.001194513149094122810, 0.001592684198792158976, 0.001990855248490195142, 0.002389026298188230875, 0.002787197347886267041, 0.003185368397584303207 ),
 .UNSPECIFIED. ) ;
#9271 =( NAMED_UNIT ( * ) SI_UNIT ( $, .STERADIAN. ) SOLID_ANGLE_UNIT ( ) );
#9272 = EDGE_CURVE ( 'NONE', #13191, #4430, #12597, .T. ) ;
#9273 = DIRECTION ( 'NONE',  ( -0.4873681696970816879, -0.8731965799097684000, 0.000000000000000000 ) ) ;
#9274 = EDGE_CURVE ( 'NONE', #7454, #14684, #1554, .T. ) ;
#9275 = CARTESIAN_POINT ( 'NONE',  ( -193.9023367725753815, 141.7188637290702502, -0.4547266291960752049 ) ) ;
#9276 = DIRECTION ( 'NONE',  ( 0.000000000000000000, 0.000000000000000000, 1.000000000000000000 ) ) ;
#9277 = EDGE_LOOP ( 'NONE', ( #698, #15389, #4129, #5975 ) ) ;
#9278 = CARTESIAN_POINT ( 'NONE',  ( -191.1563096742665380, 133.0698578461479826, -5.230826428279597984 ) ) ;
#9279 = CARTESIAN_POINT ( 'NONE',  ( 203.9760488007458719, 51.69772753023573131, 0.6543994141905550288 ) ) ;
#9280 = VERTEX_POINT ( 'NONE', #11345 ) ;
#9281 = LINE ( 'NONE', #11726, #10579 ) ;
#9282 = FACE_OUTER_BOUND ( 'NONE', #13747, .T. ) ;
#9283 = DIRECTION ( 'NONE',  ( -0.000000000000000000, 1.000000000000000000, -0.000000000000000000 ) ) ;
#9284 = TOROIDAL_SURFACE ( 'NONE', #12542, 1.000000000000000000, 0.5000000000000000000 ) ;
#9285 = ORIENTED_EDGE ( 'NONE', *, *, #1422, .T. ) ;
#9286 = TOROIDAL_SURFACE ( 'NONE', #6764, 4.799128011492294732, 1.499999999999997113 ) ;
#9287 = CARTESIAN_POINT ( 'NONE',  ( -76.00000000000001421, 13.40307322461932493, -2.295403246091865412 ) ) ;
#9288 = ORIENTED_EDGE ( 'NONE', *, *, #10791, .F. ) ;
#9289 = CARTESIAN_POINT ( 'NONE',  ( 178.0000000000000853, 15.03993994372673804, 38.07518420361041933 ) ) ;
#9290 = CARTESIAN_POINT ( 'NONE',  ( -204.1871669930114024, 142.4247710585700020, 9.578254705571842109 ) ) ;
#9291 = DIRECTION ( 'NONE',  ( 0.000000000000000000, -1.486905836551548832E-16, 1.000000000000000000 ) ) ;
#9292 = CARTESIAN_POINT ( 'NONE',  ( -35.99999999999995026, 59.53993994372674337, 15.00000000000139977 ) ) ;
#9293 = PRODUCT_DEFINITION_SHAPE ( 'NONE', 'NONE',  #15621 ) ;
#9294 = EDGE_LOOP ( 'NONE', ( #9122, #14511 ) ) ;
#9295 = CARTESIAN_POINT ( 'NONE',  ( 190.0000000000000568, 15.03993994372673804, 24.94742576086838781 ) ) ;
#9296 = AXIS2_PLACEMENT_3D ( 'NONE', #12951, #15076, #2139 ) ;
#9297 = VERTEX_POINT ( 'NONE', #11426 ) ;
#9298 = ORIENTED_EDGE ( 'NONE', *, *, #9420, .T. ) ;
#9299 = LINE ( 'NONE', #6707, #10781 ) ;
#9300 = CARTESIAN_POINT ( 'NONE',  ( -157.6477983077465694, 110.1970436846185208, -4.548387523817069678 ) ) ;
#9301 = ORIENTED_EDGE ( 'NONE', *, *, #8871, .F. ) ;
#9302 = EDGE_CURVE ( 'NONE', #13002, #11614, #590, .T. ) ;
#9303 = DIRECTION ( 'NONE',  ( 1.000000000000000000, 0.000000000000000000, 0.000000000000000000 ) ) ;
#9304 = FACE_OUTER_BOUND ( 'NONE', #1915, .T. ) ;
#9305 = CARTESIAN_POINT ( 'NONE',  ( -221.4728790919188270, 150.4357845221465482, -4.967023597482887354 ) ) ;
#9306 = DIRECTION ( 'NONE',  ( 0.000000000000000000, 0.000000000000000000, -1.000000000000000000 ) ) ;
#9307 = DIRECTION ( 'NONE',  ( 0.000000000000000000, 0.000000000000000000, -1.000000000000000000 ) ) ;
#9308 = VECTOR ( 'NONE', #6648, 1000.000000000000000 ) ;
#9309 = DIRECTION ( 'NONE',  ( -0.000000000000000000, -0.000000000000000000, -1.000000000000000000 ) ) ;
#9310 = DIRECTION ( 'NONE',  ( -1.000000000000000000, 0.000000000000000000, 0.000000000000000000 ) ) ;
#9311 = VECTOR ( 'NONE', #15019, 1000.000000000000000 ) ;
#9312 = EDGE_CURVE ( 'NONE', #7692, #5257, #3805, .T. ) ;
#9313 = FACE_BOUND ( 'NONE', #13169, .T. ) ;
#9314 = EDGE_LOOP ( 'NONE', ( #11871, #7875 ) ) ;
#9315 = DIRECTION ( 'NONE',  ( -0.000000000000000000, -0.000000000000000000, 1.000000000000000000 ) ) ;
#9316 = ORIENTED_EDGE ( 'NONE', *, *, #6340, .F. ) ;
#9317 = DIRECTION ( 'NONE',  ( 0.000000000000000000, 0.9902680687415713612, -0.1391731009600582492 ) ) ;
#9318 = CARTESIAN_POINT ( 'NONE',  ( -70.00000000000000000, -181.3058001507315566, 77.95141194869098911 ) ) ;
#9319 = ORIENTED_EDGE ( 'NONE', *, *, #4917, .F. ) ;
#9320 = AXIS2_PLACEMENT_3D ( 'NONE', #14234, #11567, #8193 ) ;
#9321 = DIRECTION ( 'NONE',  ( 1.000000000000000000, 1.224646799147353207E-16, 1.062211776130383646E-32 ) ) ;
#9322 = DIRECTION ( 'NONE',  ( -0.000000000000000000, -0.000000000000000000, 1.000000000000000000 ) ) ;
#9323 = AXIS2_PLACEMENT_3D ( 'NONE', #2562, #10939, #9512 ) ;
#9324 = CIRCLE ( 'NONE', #6557, 4.499999999999950262 ) ;
#9325 = CARTESIAN_POINT ( 'NONE',  ( -63.50000000000002842, 17.53993994372673626, 52.49999999999997868 ) ) ;
#9326 = ORIENTED_EDGE ( 'NONE', *, *, #14410, .F. ) ;
#9327 = TOROIDAL_SURFACE ( 'NONE', #7830, 1.000000000000000000, 0.5000000000000000000 ) ;
#9328 = ORIENTED_EDGE ( 'NONE', *, *, #10129, .F. ) ;
#9329 = CIRCLE ( 'NONE', #6566, 5.400000000000019007 ) ;
#9330 = CARTESIAN_POINT ( 'NONE',  ( 211.8745662956760896, 42.53653439883859022, -6.011979689023970508 ) ) ;
#9332 = EDGE_CURVE ( 'NONE', #6993, #12750, #247, .T. ) ;
#9331 = EDGE_CURVE ( 'NONE', #11744, #2137, #5263, .T. ) ;
#9333 = FILL_AREA_STYLE ('',( #10830 ) ) ;
#9334 = ORIENTED_EDGE ( 'NONE', *, *, #14428, .F. ) ;
#9335 = LINE ( 'NONE', #8165, #11743 ) ;
#9336 = CARTESIAN_POINT ( 'NONE',  ( 0.09566599640799207382, -2.915698366337646341, 0.4498622899576191214 ) ) ;
#9337 = CARTESIAN_POINT ( 'NONE',  ( -70.00000000000000000, -179.3058001507315566, -39.95141194869120937 ) ) ;
#9338 = EDGE_LOOP ( 'NONE', ( #8258, #14571, #424, #6729 ) ) ;
#9339 = EDGE_CURVE ( 'NONE', #6971, #2984, #6831, .T. ) ;
#9340 = ORIENTED_EDGE ( 'NONE', *, *, #1026, .F. ) ;
#9341 = CARTESIAN_POINT ( 'NONE',  ( -76.00000000000004263, 15.17911304468679745, 25.93769382960994818 ) ) ;
#9342 = CARTESIAN_POINT ( 'NONE',  ( 175.9483885134608272, -178.8058001507315566, 65.31842631998698323 ) ) ;
#9343 = ORIENTED_EDGE ( 'NONE', *, *, #5178, .F. ) ;
#9344 = DIRECTION ( 'NONE',  ( -3.965082230804130220E-16, 4.956352788505162775E-17, -1.000000000000000000 ) ) ;
#9345 = CARTESIAN_POINT ( 'NONE',  ( -76.00000000000001421, 14.90076684276668040, -2.084916134869001958 ) ) ;
#9346 = VECTOR ( 'NONE', #4786, 1000.000000000000000 ) ;
#9347 = CYLINDRICAL_SURFACE ( 'NONE', #11104, 1.700000000000007061 ) ;
#9348 = EDGE_CURVE ( 'NONE', #9928, #7532, #6337, .T. ) ;
#9349 = AXIS2_PLACEMENT_3D ( 'NONE', #6655, #7598, #8773 ) ;
#9350 = ORIENTED_EDGE ( 'NONE', *, *, #6508, .F. ) ;
#9351 = LINE ( 'NONE', #10765, #12478 ) ;
#9352 = AXIS2_PLACEMENT_3D ( 'NONE', #10850, #14225, #3422 ) ;
#9353 = DIRECTION ( 'NONE',  ( -0.000000000000000000, 1.000000000000000000, -0.000000000000000000 ) ) ;
#9354 = EDGE_LOOP ( 'NONE', ( #15477, #7724, #10924, #14866 ) ) ;
#9355 = CARTESIAN_POINT ( 'NONE',  ( -174.6098962832414827, 120.3911030166530054, -4.778074536717329401 ) ) ;
#9356 = CARTESIAN_POINT ( 'NONE',  ( 209.5364819485449175, 48.08777744531177945, -8.760749929847346351 ) ) ;
#9357 = ADVANCED_FACE ( 'NONE', ( #13471 ), #1465, .T. ) ;
#9358 = ORIENTED_EDGE ( 'NONE', *, *, #4596, .T. ) ;
#9359 = CARTESIAN_POINT ( 'NONE',  ( -4.116580123655898169E-16, 2.516314840832717170, 1.141614847838143820 ) ) ;
#9360 = FACE_OUTER_BOUND ( 'NONE', #12386, .T. ) ;
#9361 = AXIS2_PLACEMENT_3D ( 'NONE', #48, #4885, #14495 ) ;
#9362 = CARTESIAN_POINT ( 'NONE',  ( 164.0000000000000568, 59.53993994372674337, 15.00000000000000355 ) ) ;
#9363 = VECTOR ( 'NONE', #13139, 1000.000000000000000 ) ;
#9364 = EDGE_CURVE ( 'NONE', #555, #8585, #4805, .T. ) ;
#9365 = ORIENTED_EDGE ( 'NONE', *, *, #8034, .T. ) ;
#9366 = DIRECTION ( 'NONE',  ( 0.000000000000000000, 0.000000000000000000, 1.000000000000000000 ) ) ;
#9367 = CARTESIAN_POINT ( 'NONE',  ( 190.0000000000000853, -178.7362136002515172, 52.68580191161573367 ) ) ;
#9368 = DIRECTION ( 'NONE',  ( -0.000000000000000000, 1.000000000000000000, -0.000000000000000000 ) ) ;
#9369 = EDGE_LOOP ( 'NONE', ( #13626, #10744, #239, #8506 ) ) ;
#9370 = DIRECTION ( 'NONE',  ( 1.000000000000000000, 0.000000000000000000, 0.000000000000000000 ) ) ;
#9371 = CARTESIAN_POINT ( 'NONE',  ( -187.3366327499677197, 121.3409432500951937, 5.434137442415932107 ) ) ;
#9372 = CARTESIAN_POINT ( 'NONE',  ( -85.99999999999994316, 64.53993994372673626, 16.70000000000174012 ) ) ;
#9373 = CARTESIAN_POINT ( 'NONE',  ( 224.0000000000000853, 19.53993994372674337, 9.999999999999998224 ) ) ;
#9375 = DIRECTION ( 'NONE',  ( 0.000000000000000000, 0.000000000000000000, 1.000000000000000000 ) ) ;
#9374 = AXIS2_PLACEMENT_3D ( 'NONE', #10577, #4722, #8151 ) ;
#9376 = VERTEX_POINT ( 'NONE', #5428 ) ;
#9377 = ORIENTED_EDGE ( 'NONE', *, *, #15360, .F. ) ;
#9378 = AXIS2_PLACEMENT_3D ( 'NONE', #10945, #1293, #12188 ) ;
#9379 = DIRECTION ( 'NONE',  ( -0.000000000000000000, 1.000000000000000000, -0.000000000000000000 ) ) ;
#9380 = DIRECTION ( 'NONE',  ( -1.000000000000000000, 0.000000000000000000, 0.000000000000000000 ) ) ;
#9381 = CARTESIAN_POINT ( 'NONE',  ( -155.6477983077465410, 110.1970436846185066, 0.000000000000000000 ) ) ;
#9382 = DIRECTION ( 'NONE',  ( -0.000000000000000000, 1.000000000000000000, -0.000000000000000000 ) ) ;
#9383 = CARTESIAN_POINT ( 'NONE',  ( -223.1352769555567193, 147.4573377970056072, -4.744530085462122848 ) ) ;
#9384 = CARTESIAN_POINT ( 'NONE',  ( -223.0197145437652466, 143.2174277694208513, 6.812014755452646675 ) ) ;
#9385 = CARTESIAN_POINT ( 'NONE',  ( 200.1062858801516597, 40.86394065090267702, -20.00000000000000000 ) ) ;
#9386 = VECTOR ( 'NONE', #9403, 1000.000000000000000 ) ;
#9387 = LINE ( 'NONE', #15210, #6923 ) ;
#9388 = FACE_OUTER_BOUND ( 'NONE', #11380, .T. ) ;
#9389 = DIRECTION ( 'NONE',  ( 1.000000000000000000, 0.000000000000000000, 0.000000000000000000 ) ) ;
#9390 = ORIENTED_EDGE ( 'NONE', *, *, #8098, .T. ) ;
#9391 = ORIENTED_EDGE ( 'NONE', *, *, #14681, .T. ) ;
#9392 = DIRECTION ( 'NONE',  ( 1.000000000000000000, 0.000000000000000000, 0.000000000000000000 ) ) ;
#9393 = DIRECTION ( 'NONE',  ( -0.000000000000000000, 1.000000000000000000, -0.000000000000000000 ) ) ;
#9394 = CARTESIAN_POINT ( 'NONE',  ( 0.4964154566687934422, -8.859816792613649739, 0.6543471694412702488 ) ) ;
#9395 = CARTESIAN_POINT ( 'NONE',  ( -167.7990583880505824, 127.5943188236592363, 2.500000001005440620 ) ) ;
#9396 = FACE_BOUND ( 'NONE', #15470, .T. ) ;
#9397 = CLOSED_SHELL ( 'NONE', ( #2856, #11280, #11985, #1364, #5786, #14528, #2574, #7127, #4217, #820, #7705, #5537, #7702, #11124, #13175, #984, #13287, #596, #9518, #9898, #3633, #7901, #10865, #12527, #10980, #13279, #2476, #14222, #10012, #83, #11446, #9503, #9752, #8180, #8274, #6245, #13596, #10774, #1151, #3565, #10991, #14602, #10640, #8323, #14840, #13070, #15013, #7785, #1220, #10469, #8887, #7464, #7750, #12699, #13583, #11676, #11358 ) ) ;
#9398 = ADVANCED_FACE ( 'NONE', ( #10549 ), #3368, .T. ) ;
#9399 = ADVANCED_FACE ( 'NONE', ( #8127 ), #2803, .F. ) ;
#9400 = ORIENTED_EDGE ( 'NONE', *, *, #5818, .F. ) ;
#9401 = VERTEX_POINT ( 'NONE', #15036 ) ;
#9402 = CARTESIAN_POINT ( 'NONE',  ( 211.9051874564029561, 39.35763625820981559, -9.133132850359100274 ) ) ;
#9403 = DIRECTION ( 'NONE',  ( -1.000000000000000000, -0.000000000000000000, -0.000000000000000000 ) ) ;
#9404 = VERTEX_POINT ( 'NONE', #9219 ) ;
#9405 = CONICAL_SURFACE ( 'NONE', #3601, 2.749999999999999112, 1.047197551196600296 ) ;
#9406 = DIRECTION ( 'NONE',  ( 1.000000000000000000, 0.000000000000000000, 0.000000000000000000 ) ) ;
#9407 = CARTESIAN_POINT ( 'NONE',  ( 172.5293059057019889, 61.25683321636181233, 5.000000000000000000 ) ) ;
#9408 = DIRECTION ( 'NONE',  ( 0.000000000000000000, 0.000000000000000000, 1.000000000000000000 ) ) ;
#9409 = VERTEX_POINT ( 'NONE', #15267 ) ;
#9410 = VERTEX_POINT ( 'NONE', #14170 ) ;
#9411 = CARTESIAN_POINT ( 'NONE',  ( 169.5018791832601721, 101.0521538385604003, 5.000000000000000000 ) ) ;
#9412 = EDGE_CURVE ( 'NONE', #9203, #11790, #5589, .T. ) ;
#9413 = DIRECTION ( 'NONE',  ( 0.000000000000000000, 0.000000000000000000, -1.000000000000000000 ) ) ;
#9414 = VECTOR ( 'NONE', #5062, 1000.000000000000000 ) ;
#9415 = ORIENTED_EDGE ( 'NONE', *, *, #12469, .F. ) ;
#9416 = DIRECTION ( 'NONE',  ( 0.000000000000000000, -0.1391731009600591096, 0.9902680687415711391 ) ) ;
#9417 = ADVANCED_FACE ( 'NONE', ( #11580, #829 ), #905, .T. ) ;
#9418 = DIRECTION ( 'NONE',  ( 0.000000000000000000, 1.000000000000000000, 0.000000000000000000 ) ) ;
#9419 = AXIS2_PLACEMENT_3D ( 'NONE', #9462, #13147, #995 ) ;
#9420 = EDGE_CURVE ( 'NONE', #6168, #12024, #2024, .T. ) ;
#9421 = EDGE_CURVE ( 'NONE', #5266, #5077, #8844, .T. ) ;
#9422 = VERTEX_POINT ( 'NONE', #7891 ) ;
#9423 = DIRECTION ( 'NONE',  ( 1.000000000000000000, -6.938893903907222067E-15, 0.000000000000000000 ) ) ;
#9424 = EDGE_LOOP ( 'NONE', ( #12554, #5211 ) ) ;
#9425 = CARTESIAN_POINT ( 'NONE',  ( 126.0806775638430253, 45.00321902537314145, 7.600000000000002309 ) ) ;
#9426 = CARTESIAN_POINT ( 'NONE',  ( -224.5811800873043182, 144.8667753680073531, 1.831365460742872209 ) ) ;
#9427 = CARTESIAN_POINT ( 'NONE',  ( 224.0000000000000853, 56.53993994372675047, 13.00000000000000178 ) ) ;
#9428 = ORIENTED_EDGE ( 'NONE', *, *, #13719, .T. ) ;
#9429 = CARTESIAN_POINT ( 'NONE',  ( -202.2493014528935475, 138.0335512477381883, -5.230826428279597096 ) ) ;
#9430 = CARTESIAN_POINT ( 'NONE',  ( 191.4069380837317453, 39.61051162384328705, -7.503330758807070566 ) ) ;
#9431 = ADVANCED_BREP_SHAPE_REPRESENTATION ( '', ( #11106, #12337 ), #6268 ) ;
#9432 = VECTOR ( 'NONE', #3986, 1000.000000000000000 ) ;
#9433 = VERTEX_POINT ( 'NONE', #10400 ) ;
#9434 = EDGE_CURVE ( 'NONE', #379, #207, #775, .T. ) ;
#9435 = EDGE_CURVE ( 'NONE', #7302, #11235, #14644, .T. ) ;
#9436 = AXIS2_PLACEMENT_3D ( 'NONE', #12050, #8513, #2584 ) ;
#9437 = FACE_OUTER_BOUND ( 'NONE', #986, .T. ) ;
#9438 = FACE_BOUND ( 'NONE', #14445, .T. ) ;
#9439 = ADVANCED_FACE ( 'NONE', ( #8042 ), #10622, .T. ) ;
#9440 = CARTESIAN_POINT ( 'NONE',  ( -151.6539382783454926, 106.2940129864185366, -4.336802791931510193 ) ) ;
#9441 = ORIENTED_EDGE ( 'NONE', *, *, #278, .F. ) ;
#9442 =( NAMED_UNIT ( * ) SI_UNIT ( $, .STERADIAN. ) SOLID_ANGLE_UNIT ( ) );
#9443 = AXIS2_PLACEMENT_3D ( 'NONE', #11299, #4475, #7023 ) ;
#9444 =( NAMED_UNIT ( * ) SI_UNIT ( $, .STERADIAN. ) SOLID_ANGLE_UNIT ( ) );
#9445 = CARTESIAN_POINT ( 'NONE',  ( 208.8186272397570349, 39.68461847005694665, -7.558035125831273682 ) ) ;
#9446 = VERTEX_POINT ( 'NONE', #4547 ) ;
#9447 = CARTESIAN_POINT ( 'NONE',  ( 190.5000000000000853, 15.03993994372673804, 24.94742576086838781 ) ) ;
#9448 = PRESENTATION_LAYER_ASSIGNMENT (  '', '', ( #2123 ) ) ;
#9449 = CARTESIAN_POINT ( 'NONE',  ( -214.6174474432871762, 135.6318802667844921, 5.434137442415934771 ) ) ;
#9450 = DIRECTION ( 'NONE',  ( -0.000000000000000000, 1.000000000000000000, -0.000000000000000000 ) ) ;
#9451 = CARTESIAN_POINT ( 'NONE',  ( 0.000000000000000000, 6.928203230275487456, 4.000000000000003553 ) ) ;
#9452 = DIRECTION ( 'NONE',  ( 0.000000000000000000, -0.1391731009600591096, 0.9902680687415711391 ) ) ;
#9453 = EDGE_CURVE ( 'NONE', #13487, #5951, #14092, .T. ) ;
#9454 = ORIENTED_EDGE ( 'NONE', *, *, #11053, .T. ) ;
#9455 = ORIENTED_EDGE ( 'NONE', *, *, #1778, .F. ) ;
#9456 = CARTESIAN_POINT ( 'NONE',  ( -70.00000000000000000, -181.3058001507315566, -41.45141194869120227 ) ) ;
#9457 = DIRECTION ( 'NONE',  ( 0.000000000000000000, 0.000000000000000000, 1.000000000000000000 ) ) ;
#9458 = AXIS2_PLACEMENT_3D ( 'NONE', #3127, #584, #1931 ) ;
#9459 = FACE_BOUND ( 'NONE', #3732, .T. ) ;
#9460 = CARTESIAN_POINT ( 'NONE',  ( -61.94838851346079167, -179.3058001507315566, 52.76585208085545275 ) ) ;
#9461 = CARTESIAN_POINT ( 'NONE',  ( -221.1031640812056764, 146.8836531993028132, -4.819768081029505602 ) ) ;
#9462 = CARTESIAN_POINT ( 'NONE',  ( 0.000000000000000000, 0.000000000000000000, 0.000000000000000000 ) ) ;
#9463 = CARTESIAN_POINT ( 'NONE',  ( 0.3157512944565224466, -3.097794232830199057, -7.999999999999979572 ) ) ;
#9464 = FACE_OUTER_BOUND ( 'NONE', #10321, .T. ) ;
#9465 = VECTOR ( 'NONE', #803, 1000.000000000000000 ) ;
#9466 = CARTESIAN_POINT ( 'NONE',  ( -167.5053995445195767, 127.4304153265770907, 2.500000001036336350 ) ) ;
#9467 = EDGE_CURVE ( 'NONE', #14786, #14360, #1860, .T. ) ;
#9468 = CARTESIAN_POINT ( 'NONE',  ( 64.00000000000005684, 64.53993994372673626, 15.00000000000070166 ) ) ;
#9469 = CARTESIAN_POINT ( 'NONE',  ( 14.00000000000004086, 64.51493994372674479, 18.50000000000105160 ) ) ;
#9470 = EDGE_LOOP ( 'NONE', ( #14991, #13419, #1748, #14673 ) ) ;
#9471 = ORIENTED_EDGE ( 'NONE', *, *, #14042, .F. ) ;
#9472 = DIRECTION ( 'NONE',  ( 0.000000000000000000, 0.000000000000000000, 1.000000000000000000 ) ) ;
#9473 = DIRECTION ( 'NONE',  ( -1.000000000000000000, -2.751328491981765035E-32, 3.965082230804130220E-16 ) ) ;
#9474 = DIRECTION ( 'NONE',  ( -0.7900120431063429871, 0.6130913241491365850, 0.000000000000000000 ) ) ;
#9475 = DIRECTION ( 'NONE',  ( 1.000000000000000000, 0.000000000000000000, 0.000000000000000000 ) ) ;
#9476 = CIRCLE ( 'NONE', #4932, 1.499999999999997780 ) ;
#9477 = VECTOR ( 'NONE', #13992, 1000.000000000000114 ) ;
#9478 = ORIENTED_EDGE ( 'NONE', *, *, #10921, .F. ) ;
#9479 = EDGE_CURVE ( 'NONE', #6496, #8326, #11816, .T. ) ;
#9480 = ORIENTED_EDGE ( 'NONE', *, *, #6061, .F. ) ;
#9481 = CARTESIAN_POINT ( 'NONE',  ( 205.3852585099181454, 47.89158942159311039, -8.629264428576009394 ) ) ;
#9482 = ADVANCED_FACE ( 'NONE', ( #15115, #9149 ), #13869, .F. ) ;
#9483 =( NAMED_UNIT ( * ) SI_UNIT ( $, .STERADIAN. ) SOLID_ANGLE_UNIT ( ) );
#9484 = ORIENTED_EDGE ( 'NONE', *, *, #10269, .F. ) ;
#9485 = DIRECTION ( 'NONE',  ( 0.8731965799097685110, -0.4873681696970816324, -0.000000000000000000 ) ) ;
#9486 = CIRCLE ( 'NONE', #129, 0.5000000000000004441 ) ;
#9487 = CYLINDRICAL_SURFACE ( 'NONE', #6078, 3.500000000000003109 ) ;
#9488 = CARTESIAN_POINT ( 'NONE',  ( -220.3531759299249302, 148.3382346779569616, 2.431557144026069928 ) ) ;
#9489 = ORIENTED_EDGE ( 'NONE', *, *, #3840, .F. ) ;
#9490 = EDGE_LOOP ( 'NONE', ( #6045, #3370, #6952, #3386 ) ) ;
#9491 = DIRECTION ( 'NONE',  ( -0.000000000000000000, -4.956352788505162775E-17, 1.000000000000000000 ) ) ;
#9492 = CARTESIAN_POINT ( 'NONE',  ( -70.00000000000000000, 17.53993994372673626, 48.99999999999997158 ) ) ;
#9493 = EDGE_LOOP ( 'NONE', ( #7450, #9377, #3603, #9608 ) ) ;
#9494 = CARTESIAN_POINT ( 'NONE',  ( -151.5230023344471704, 106.2706521918282903, 9.220837571243215791 ) ) ;
#9495 = DIRECTION ( 'NONE',  ( -5.518327896226373307E-17, 0.9902680687415712502, 0.1391731009600586100 ) ) ;
#9496 = EDGE_CURVE ( 'NONE', #8640, #5077, #746, .T. ) ;
#9497 = DIRECTION ( 'NONE',  ( 0.000000000000000000, 0.4999999999999996669, -0.8660254037844388186 ) ) ;
#9498 = CIRCLE ( 'NONE', #5959, 1.219500000000000028 ) ;
#9499 = ORIENTED_EDGE ( 'NONE', *, *, #3357, .T. ) ;
#9500 = DIRECTION ( 'NONE',  ( 1.000000000000000000, 0.000000000000000000, 0.000000000000000000 ) ) ;
#9501 = VERTEX_POINT ( 'NONE', #14479 ) ;
#9502 = DIRECTION ( 'NONE',  ( -0.000000000000000000, 1.000000000000000000, -0.000000000000000000 ) ) ;
#9503 = ADVANCED_FACE ( 'NONE', ( #11895, #3674 ), #4700, .F. ) ;
#9504 = CARTESIAN_POINT ( 'NONE',  ( -36.49899788034579018, 48.72489408690345414, 10.00000000000000178 ) ) ;
#9505 = DIRECTION ( 'NONE',  ( -0.000000000000000000, -0.000000000000000000, 1.000000000000000000 ) ) ;
#9506 = EDGE_LOOP ( 'NONE', ( #1977, #10571, #10210, #667 ) ) ;
#9507 = CARTESIAN_POINT ( 'NONE',  ( -198.7485669925355012, 144.4350871509360559, -0.4547266291960735951 ) ) ;
#9508 = CARTESIAN_POINT ( 'NONE',  ( 207.0793923465612352, 46.18607573428356972, -5.755770042397863051 ) ) ;
#9509 = VERTEX_POINT ( 'NONE', #4783 ) ;
#9510 = FACE_BOUND ( 'NONE', #1644, .T. ) ;
#9511 = LINE ( 'NONE', #7076, #1659 ) ;
#9512 = DIRECTION ( 'NONE',  ( 1.000000000000000000, 0.000000000000000000, 0.000000000000000000 ) ) ;
#9513 = ORIENTED_EDGE ( 'NONE', *, *, #7777, .T. ) ;
#9514 = DIRECTION ( 'NONE',  ( 0.000000000000000000, -1.000000000000000000, -1.156482317317871725E-16 ) ) ;
#9515 = CARTESIAN_POINT ( 'NONE',  ( 208.8124460758720033, 42.05191026284237665, -4.433604294307299298 ) ) ;
#9516 = EDGE_LOOP ( 'NONE', ( #852, #5542, #13765, #12559 ) ) ;
#9517 = CARTESIAN_POINT ( 'NONE',  ( -99.68324453533686835, 80.15913712344708131, 10.00000000000000178 ) ) ;
#9518 = ADVANCED_FACE ( 'NONE', ( #8356, #15579 ), #9763, .T. ) ;
#9519 = CARTESIAN_POINT ( 'NONE',  ( -184.7761983179757976, 119.6423109536379883, 5.434137442415926778 ) ) ;
#9522 = EDGE_CURVE ( 'NONE', #13999, #13543, #5, .T. ) ;
#9521 = ADVANCED_FACE ( 'NONE', ( #3519 ), #10875, .T. ) ;
#9520 = CARTESIAN_POINT ( 'NONE',  ( 6.399999999999999467, 4.618802153516981868, 8.000000000000007105 ) ) ;
#9523 = DIRECTION ( 'NONE',  ( -0.000000000000000000, -0.000000000000000000, 1.000000000000000000 ) ) ;
#9524 = DIRECTION ( 'NONE',  ( 0.000000000000000000, 1.486905836551548832E-16, -1.000000000000000000 ) ) ;
#9525 = VERTEX_POINT ( 'NONE', #10633 ) ;
#9526 = VERTEX_POINT ( 'NONE', #2578 ) ;
#9527 = CARTESIAN_POINT ( 'NONE',  ( -209.4367884691887980, 132.9649188877714607, 2.431555724346876168 ) ) ;
#9528 = CARTESIAN_POINT ( 'NONE',  ( -76.50000000000001421, 15.53993994372673804, 38.07518420361041933 ) ) ;
#9529 = AXIS2_PLACEMENT_3D ( 'NONE', #4826, #10674, #2534 ) ;
#9530 = CARTESIAN_POINT ( 'NONE',  ( -63.50000000000002842, 15.03993994372673804, 38.07518420361041933 ) ) ;
#9531 = DIRECTION ( 'NONE',  ( 1.000000000000000000, 0.000000000000000000, 0.000000000000000000 ) ) ;
#9532 = CARTESIAN_POINT ( 'NONE',  ( -222.0356587614904811, 145.0888860198141685, -3.948294122849004051 ) ) ;
#9533 = VECTOR ( 'NONE', #1119, 1000.000000000000000 ) ;
#9534 = DIRECTION ( 'NONE',  ( 1.000000000000000000, 0.000000000000000000, 0.000000000000000000 ) ) ;
#9535 = CARTESIAN_POINT ( 'NONE',  ( -38.29899788034579444, 48.72489408690345414, 10.00000000000000178 ) ) ;
#9536 = LINE ( 'NONE', #1157, #11296 ) ;
#9537 = CARTESIAN_POINT ( 'NONE',  ( -156.8971783069440278, 109.2193490945657430, 9.199440363476590221 ) ) ;
#9538 = AXIS2_PLACEMENT_3D ( 'NONE', #1471, #7493, #12217 ) ;
#9539 = CARTESIAN_POINT ( 'NONE',  ( 0.1090894304641042839, -1.847874265840313335, 2.299387885565523870 ) ) ;
#9540 = DIRECTION ( 'NONE',  ( -0.000000000000000000, -0.000000000000000000, 1.000000000000000000 ) ) ;
#9541 = CIRCLE ( 'NONE', #5781, 0.5000000000000004441 ) ;
#9542 = EDGE_LOOP ( 'NONE', ( #13353, #1965 ) ) ;
#9543 = VECTOR ( 'NONE', #6074, 1000.000000000000000 ) ;
#9544 = ORIENTED_EDGE ( 'NONE', *, *, #12628, .T. ) ;
#9545 = LINE ( 'NONE', #14191, #200 ) ;
#9546 = DIRECTION ( 'NONE',  ( -1.000000000000000000, 0.000000000000000000, 0.000000000000000000 ) ) ;
#9547 = DIRECTION ( 'NONE',  ( 0.000000000000000000, -1.734723475976808672E-15, 1.000000000000000000 ) ) ;
#9548 = SURFACE_STYLE_FILL_AREA ( #932 ) ;
#9549 = CARTESIAN_POINT ( 'NONE',  ( 0.000000000000000000, 3.175426480542944407, -3.252606517456511330E-16 ) ) ;
#9550 = PRODUCT_DEFINITION_SHAPE ( 'NONE', 'NONE',  #8944 ) ;
#9551 = LINE ( 'NONE', #15239, #6313 ) ;
#9552 = CARTESIAN_POINT ( 'NONE',  ( -169.9318100387881714, 128.7846982781319412, 2.500000000781056997 ) ) ;
#9553 = AXIS2_PLACEMENT_3D ( 'NONE', #9411, #14209, #10443 ) ;
#9554 = ORIENTED_EDGE ( 'NONE', *, *, #6815, .F. ) ;
#9555 = VECTOR ( 'NONE', #3907, 1000.000000000000114 ) ;
#9556 = EDGE_CURVE ( 'NONE', #12092, #10399, #1070, .T. ) ;
#9557 = ORIENTED_EDGE ( 'NONE', *, *, #12361, .T. ) ;
#9558 = CARTESIAN_POINT ( 'NONE',  ( 198.8104769829885754, 49.54338459298288200, -5.250705761417654216 ) ) ;
#9559 = ORIENTED_EDGE ( 'NONE', *, *, #1415, .T. ) ;
#9560 = DIRECTION ( 'NONE',  ( 0.000000000000000000, 0.000000000000000000, 1.000000000000000000 ) ) ;
#9561 = CARTESIAN_POINT ( 'NONE',  ( -223.9066929173374376, 146.0752250096516605, 8.917334695103006581 ) ) ;
#9562 = EDGE_LOOP ( 'NONE', ( #11164, #5096, #172, #2696 ) ) ;
#9563 = AXIS2_PLACEMENT_3D ( 'NONE', #9088, #10419, #12852 ) ;
#9564 = ORIENTED_EDGE ( 'NONE', *, *, #4283, .T. ) ;
#9565 = DIRECTION ( 'NONE',  ( 0.000000000000000000, -1.000000000000000000, 0.000000000000000000 ) ) ;
#9566 = DIRECTION ( 'NONE',  ( 0.000000000000000000, -1.000000000000000000, -1.156482317317871478E-16 ) ) ;
#9567 = AXIS2_PLACEMENT_3D ( 'NONE', #92, #1132, #9750 ) ;
#9568 = VECTOR ( 'NONE', #8183, 1000.000000000000000 ) ;
#9569 = ORIENTED_EDGE ( 'NONE', *, *, #9636, .T. ) ;
#9570 = DIRECTION ( 'NONE',  ( -0.8731965799097680669, 0.4873681696970824651, 0.000000000000000000 ) ) ;
#9571 = EDGE_CURVE ( 'NONE', #3949, #12821, #9607, .T. ) ;
#9572 = CARTESIAN_POINT ( 'NONE',  ( 114.0000000000000568, 62.13993994372673768, 15.00000000000035172 ) ) ;
#9573 = CIRCLE ( 'NONE', #6804, 1.499999999999997558 ) ;
#9574 = CIRCLE ( 'NONE', #13334, 3.500000000000004885 ) ;
#9575 = EDGE_LOOP ( 'NONE', ( #11609, #11453, #7685, #3653, #12640 ) ) ;
#9576 = LINE ( 'NONE', #9658, #13798 ) ;
#9577 = EDGE_LOOP ( 'NONE', ( #7120, #9106 ) ) ;
#9578 = CARTESIAN_POINT ( 'NONE',  ( 200.1062858801516597, 40.86394065090267702, -20.00000000000000000 ) ) ;
#9579 = DIRECTION ( 'NONE',  ( 0.000000000000000000, 0.000000000000000000, 1.000000000000000000 ) ) ;
#9580 = CARTESIAN_POINT ( 'NONE',  ( -150.6128662652177752, 107.8929640959227356, -4.950117075408072331 ) ) ;
#9581 = VECTOR ( 'NONE', #4873, 1000.000000000000000 ) ;
#9582 = ORIENTED_EDGE ( 'NONE', *, *, #14030, .F. ) ;
#9583 = EDGE_LOOP ( 'NONE', ( #10968, #10827, #13172, #12318 ) ) ;
#9584 = CARTESIAN_POINT ( 'NONE',  ( -198.5633888957220563, 144.7754908190922549, 1.515441477536285442 ) ) ;
#9585 = CARTESIAN_POINT ( 'NONE',  ( 190.6749524420355328, 33.64372802412135144, -4.260924496400990691 ) ) ;
#9586 = CIRCLE ( 'NONE', #9097, 0.5000000000000004441 ) ;
#9587 = VERTEX_POINT ( 'NONE', #14404 ) ;
#9588 = CIRCLE ( 'NONE', #14357, 338.5619230110239641 ) ;
#9589 = DIRECTION ( 'NONE',  ( 0.000000000000000000, 0.000000000000000000, -1.000000000000000000 ) ) ;
#9590 = DIRECTION ( 'NONE',  ( -5.518327896226365911E-17, -0.9902680687415714722, 0.1391731009600582769 ) ) ;
#9591 = CARTESIAN_POINT ( 'NONE',  ( 71.96535645333923981, 38.79159067395544014, 7.600000000000002309 ) ) ;
#9592 = EDGE_CURVE ( 'NONE', #10091, #15368, #7089, .T. ) ;
#9593 = CIRCLE ( 'NONE', #4536, 0.5000000000000004441 ) ;
#9594 = ORIENTED_EDGE ( 'NONE', *, *, #4198, .T. ) ;
#9595 = AXIS2_PLACEMENT_3D ( 'NONE', #8211, #12991, #10636 ) ;
#9596 = SHAPE_DEFINITION_REPRESENTATION ( #4104, #11876 ) ;
#9597 = AXIS2_PLACEMENT_3D ( 'NONE', #15028, #4215, #14950 ) ;
#9598 = FILL_AREA_STYLE ('',( #5962 ) ) ;
#9599 = CARTESIAN_POINT ( 'NONE',  ( 203.0658429208174880, 48.83360436048501896, -0.9158339742359169477 ) ) ;
#9600 = ORIENTED_EDGE ( 'NONE', *, *, #1181, .T. ) ;
#9601 = DIRECTION ( 'NONE',  ( 0.000000000000000000, 0.000000000000000000, -1.000000000000000000 ) ) ;
#9602 = CARTESIAN_POINT ( 'NONE',  ( 51.07686401294030532, 368.7106150007013525, 10.00000000000000178 ) ) ;
#9603 = CARTESIAN_POINT ( 'NONE',  ( -194.4337897068680547, 127.2572260587109554, 1.515400478619095992 ) ) ;
#9604 = DIRECTION ( 'NONE',  ( -1.000000000000000000, 0.000000000000000000, 0.000000000000000000 ) ) ;
#9605 = ORIENTED_EDGE ( 'NONE', *, *, #15503, .T. ) ;
#9606 = CARTESIAN_POINT ( 'NONE',  ( -217.2220691230952525, 140.9637235289241062, 7.918248976830628116 ) ) ;
#9607 = LINE ( 'NONE', #1300, #3308 ) ;
#9608 = ORIENTED_EDGE ( 'NONE', *, *, #15132, .T. ) ;
#9609 = VERTEX_POINT ( 'NONE', #4869 ) ;
#9610 = CIRCLE ( 'NONE', #14869, 1.700000000000007061 ) ;
#9611 = CARTESIAN_POINT ( 'NONE',  ( -70.00000000000000000, -201.3058001507315566, 74.95141194869098911 ) ) ;
#9612 = DIRECTION ( 'NONE',  ( 0.000000000000000000, -1.000000000000000000, 0.000000000000000000 ) ) ;
#9613 = EDGE_CURVE ( 'NONE', #4660, #12466, #6133, .T. ) ;
#9614 = CIRCLE ( 'NONE', #2541, 1.499999999999997780 ) ;
#9615 = DIRECTION ( 'NONE',  ( -0.000000000000000000, -0.9902680687415711391, -0.1391731009600592484 ) ) ;
#9616 = PLANE ( 'NONE',  #10503 ) ;
#9617 = CARTESIAN_POINT ( 'NONE',  ( -63.50000000000002842, -178.9449732516916072, 64.32815825124541220 ) ) ;
#9618 = ADVANCED_FACE ( 'NONE', ( #3602 ), #14934, .T. ) ;
#9619 = CARTESIAN_POINT ( 'NONE',  ( -221.2401356301573685, 146.6832912211113467, 9.651641063605101323 ) ) ;
#9620 = DIRECTION ( 'NONE',  ( -0.9741547192086867923, 0.2258817899775115157, 1.688901894271609290E-28 ) ) ;
#9621 = EDGE_CURVE ( 'NONE', #10088, #11744, #469, .T. ) ;
#9622 = AXIS2_PLACEMENT_3D ( 'NONE', #5393, #6816, #13826 ) ;
#9623 = CYLINDRICAL_SURFACE ( 'NONE', #13461, 0.4999999999999996114 ) ;
#9624 = DIRECTION ( 'NONE',  ( -0.000000000000000000, -1.000000000000000000, -6.938893903907222067E-15 ) ) ;
#9625 = CARTESIAN_POINT ( 'NONE',  ( 190.5000000000000568, -178.8058001507315566, -17.19066787724516843 ) ) ;
#9626 = VERTEX_POINT ( 'NONE', #9904 ) ;
#9627 = ORIENTED_EDGE ( 'NONE', *, *, #3798, .T. ) ;
#9628 = CARTESIAN_POINT ( 'NONE',  ( 178.0000000000000853, 14.97035339324670744, 37.58005016923963382 ) ) ;
#9629 = CARTESIAN_POINT ( 'NONE',  ( -165.1793164425202178, 126.1324870151522504, 2.431557144026069928 ) ) ;
#9630 = CARTESIAN_POINT ( 'NONE',  ( 171.7208925888976978, 62.57671370024034729, -0.9107274384406881529 ) ) ;
#9631 = DIRECTION ( 'NONE',  ( 1.000000000000000000, 0.000000000000000000, 0.000000000000000000 ) ) ;
#9632 = CARTESIAN_POINT ( 'NONE',  ( 193.3006371371548369, 56.51400776751751920, 5.000000000000000000 ) ) ;
#9633 = VECTOR ( 'NONE', #13101, 1000.000000000000000 ) ;
#9634 = DIRECTION ( 'NONE',  ( 0.000000000000000000, 0.000000000000000000, 1.000000000000000000 ) ) ;
#9635 = DIRECTION ( 'NONE',  ( 0.7071067811864983899, 0.000000000000000000, 0.7071067811865966446 ) ) ;
#9636 = EDGE_CURVE ( 'NONE', #3200, #4933, #8369, .T. ) ;
#9637 = EDGE_CURVE ( 'NONE', #15023, #1328, #10053, .T. ) ;
#9638 = CIRCLE ( 'NONE', #4841, 0.5000000000000000000 ) ;
#9639 = VERTEX_POINT ( 'NONE', #13355 ) ;
#9640 = ORIENTED_EDGE ( 'NONE', *, *, #4702, .T. ) ;
#9641 = CARTESIAN_POINT ( 'NONE',  ( 207.0671064858421744, 46.21029813590134694, -8.754270687730807410 ) ) ;
#9642 = EDGE_LOOP ( 'NONE', ( #2057, #403, #6059, #8788 ) ) ;
#9643 = AXIS2_PLACEMENT_3D ( 'NONE', #11659, #5581, #816 ) ;
#9644 = CARTESIAN_POINT ( 'NONE',  ( -225.4895753176805044, 143.2392427187964188, 4.987127499475484171 ) ) ;
#9645 = VERTEX_POINT ( 'NONE', #2558 ) ;
#9646 = ORIENTED_EDGE ( 'NONE', *, *, #364, .F. ) ;
#9647 = CARTESIAN_POINT ( 'NONE',  ( 190.5000000000000568, -179.3058001507315566, -51.45141194869120227 ) ) ;
#9648 = CIRCLE ( 'NONE', #8645, 0.9999999999999991118 ) ;
#9649 = DIRECTION ( 'NONE',  ( 0.000000000000000000, 0.000000000000000000, 1.000000000000000000 ) ) ;
#9650 = EDGE_CURVE ( 'NONE', #1731, #14876, #304, .T. ) ;
#9651 = ORIENTED_EDGE ( 'NONE', *, *, #6734, .F. ) ;
#9652 = CARTESIAN_POINT ( 'NONE',  ( -150.4086188282876719, 107.1411652488047253, 9.691934182417341503 ) ) ;
#9653 = CARTESIAN_POINT ( 'NONE',  ( 17.41029453487719181, 40.04259805664093363, 9.975000000000001421 ) ) ;
#9654 = FACE_OUTER_BOUND ( 'NONE', #13438, .T. ) ;
#9655 = AXIS2_PLACEMENT_3D ( 'NONE', #7601, #10429, #13974 ) ;
#9656 = ORIENTED_EDGE ( 'NONE', *, *, #9209, .T. ) ;
#9657 = DIRECTION ( 'NONE',  ( -0.000000000000000000, 0.000000000000000000, 1.000000000000000000 ) ) ;
#9658 = CARTESIAN_POINT ( 'NONE',  ( -157.8787660911425803, 118.6941998492684149, 5.000000000000000000 ) ) ;
#9659 = ORIENTED_EDGE ( 'NONE', *, *, #2387, .T. ) ;
#9660 = DIRECTION ( 'NONE',  ( 0.8731965799097684000, -0.4873681696970816324, -0.000000000000000000 ) ) ;
#9661 = DIRECTION ( 'NONE',  ( 1.000000000000000000, 2.751328491981765035E-32, -3.965082230804130220E-16 ) ) ;
#9662 = EDGE_CURVE ( 'NONE', #14434, #7084, #10371, .T. ) ;
#9663 = LINE ( 'NONE', #4998, #4515 ) ;
#9664 = EDGE_LOOP ( 'NONE', ( #14200, #12726, #5571, #6538, #4377 ) ) ;
#9665 = ORIENTED_EDGE ( 'NONE', *, *, #12580, .F. ) ;
#9666 = CARTESIAN_POINT ( 'NONE',  ( -182.2196890910978482, 130.3369809632412739, -4.640918829492416187 ) ) ;
#9667 = CARTESIAN_POINT ( 'NONE',  ( 198.9643688939780191, 32.15902683440354082, -3.879216492611309519 ) ) ;
#9668 = EDGE_LOOP ( 'NONE', ( #2550, #6111, #7755, #11063 ) ) ;
#9669 = CIRCLE ( 'NONE', #5124, 0.5000000000000004441 ) ;
#9670 = VECTOR ( 'NONE', #3304, 1000.000000000000000 ) ;
#9671 = CYLINDRICAL_SURFACE ( 'NONE', #2767, 0.5000000000000004441 ) ;
#9672 = CYLINDRICAL_SURFACE ( 'NONE', #2151, 0.4999999999999996114 ) ;
#9673 = DIRECTION ( 'NONE',  ( 1.000000000000000000, 2.751328491981765035E-32, -3.965082230804130220E-16 ) ) ;
#9674 = MECHANICAL_DESIGN_GEOMETRIC_PRESENTATION_REPRESENTATION (  '', ( #13443 ), #2616 ) ;
#9675 = ORIENTED_EDGE ( 'NONE', *, *, #9725, .F. ) ;
#9676 = EDGE_CURVE ( 'NONE', #649, #3946, #4818, .T. ) ;
#9677 = CARTESIAN_POINT ( 'NONE',  ( 194.7691866843436799, 33.87697957786221536, -2.559886773443665220 ) ) ;
#9678 = VERTEX_POINT ( 'NONE', #13911 ) ;
#9679 = DIRECTION ( 'NONE',  ( 0.000000000000000000, 0.000000000000000000, 1.000000000000000000 ) ) ;
#9680 = CARTESIAN_POINT ( 'NONE',  ( -142.5801316981433615, 96.86001897250537240, 5.000000000000000000 ) ) ;
#9681 = CIRCLE ( 'NONE', #3883, 1.499999999999997780 ) ;
#9682 = CARTESIAN_POINT ( 'NONE',  ( -217.9748787080196450, 139.5740753954225966, -0.4555467707853197989 ) ) ;
#9683 = DIRECTION ( 'NONE',  ( -1.000000000000000000, 0.000000000000000000, 0.000000000000000000 ) ) ;
#9684 = ORIENTED_EDGE ( 'NONE', *, *, #11169, .F. ) ;
#9685 = CARTESIAN_POINT ( 'NONE',  ( -192.4722482905459344, 130.7344553107722902, 9.577123744044227394 ) ) ;
#9686 = DIRECTION ( 'NONE',  ( 0.000000000000000000, 8.673617379884035472E-17, -1.000000000000000000 ) ) ;
#9687 = AXIS2_PLACEMENT_3D ( 'NONE', #9694, #11028, #1152 ) ;
#9688 = ORIENTED_EDGE ( 'NONE', *, *, #4556, .T. ) ;
#9689 = EDGE_LOOP ( 'NONE', ( #14928, #9181, #2646 ) ) ;
#9690 = LINE ( 'NONE', #14482, #6323 ) ;
#9691 = CARTESIAN_POINT ( 'NONE',  ( 0.1317522424471971043, 1.959574484719836196, -7.999999999999977796 ) ) ;
#9692 = EDGE_CURVE ( 'NONE', #5257, #14252, #2552, .T. ) ;
#9693 = VECTOR ( 'NONE', #11820, 1000.000000000000000 ) ;
#9694 = CARTESIAN_POINT ( 'NONE',  ( -85.27455057502459113, 65.19100426474074084, 5.000000000000000000 ) ) ;
#9695 = CARTESIAN_POINT ( 'NONE',  ( 70.26535645333922275, 38.79159067395544014, 0.000000000000000000 ) ) ;
#9696 = EDGE_CURVE ( 'NONE', #3064, #14554, #3564, .T. ) ;
#9697 = CARTESIAN_POINT ( 'NONE',  ( -223.3922821272916508, 142.4404936614456574, -0.2381634666249608234 ) ) ;
#9698 = CIRCLE ( 'NONE', #7194, 0.5000000000000001110 ) ;
#9699 = CARTESIAN_POINT ( 'NONE',  ( -223.5483852270401712, 142.1543297243506458, 4.029429640195547613 ) ) ;
#9700 = DIRECTION ( 'NONE',  ( -0.000000000000000000, -0.000000000000000000, 1.000000000000000000 ) ) ;
#9701 = CARTESIAN_POINT ( 'NONE',  ( 185.1062858801516882, 25.86394065090268057, 18.00000000000000355 ) ) ;
#9702 = CARTESIAN_POINT ( 'NONE',  ( -201.8658614229783268, 146.6084512934502584, 2.500000000000000000 ) ) ;
#9703 = DIRECTION ( 'NONE',  ( 1.000000000000000000, 0.000000000000000000, 0.000000000000000000 ) ) ;
#9704 = DIRECTION ( 'NONE',  ( 1.000000000000000000, 0.000000000000000000, 0.000000000000000000 ) ) ;
#9705 = ORIENTED_EDGE ( 'NONE', *, *, #15254, .F. ) ;
#9706 = AXIS2_PLACEMENT_3D ( 'NONE', #8293, #5184, #3921 ) ;
#9707 = EDGE_CURVE ( 'NONE', #14322, #8410, #11638, .T. ) ;
#9708 = VERTEX_POINT ( 'NONE', #8955 ) ;
#9709 = DIRECTION ( 'NONE',  ( 0.000000000000000000, 0.000000000000000000, 1.000000000000000000 ) ) ;
#9710 = DIRECTION ( 'NONE',  ( 0.8731965799097690661, -0.4873681696970805222, 0.000000000000000000 ) ) ;
#9711 = CARTESIAN_POINT ( 'NONE',  ( -35.99999999999995026, 64.53993994372673626, 15.00000000000139977 ) ) ;
#9712 = DIRECTION ( 'NONE',  ( 0.000000000000000000, -1.000000000000000000, -1.156482317317871478E-16 ) ) ;
#9713 = LINE ( 'NONE', #14503, #12511 ) ;
#9714 = PLANE ( 'NONE',  #13857 ) ;
#9715 = CARTESIAN_POINT ( 'NONE',  ( 14.00000000000004086, 62.13993994372673768, 15.00000000000104983 ) ) ;
#9716 = EDGE_LOOP ( 'NONE', ( #621, #10955, #7946, #3172 ) ) ;
#9717 = AXIS2_PLACEMENT_3D ( 'NONE', #6366, #6444, #14860 ) ;
#9718 = ORIENTED_EDGE ( 'NONE', *, *, #13880, .F. ) ;
#9719 = CARTESIAN_POINT ( 'NONE',  ( -224.5811800873043182, 144.8667753680073531, 1.831365460742872209 ) ) ;
#9720 = ORIENTED_EDGE ( 'NONE', *, *, #4164, .T. ) ;
#9721 = EDGE_CURVE ( 'NONE', #7716, #3571, #4307, .T. ) ;
#9722 = EDGE_CURVE ( 'NONE', #14048, #12371, #4352, .T. ) ;
#9724 = B_SPLINE_CURVE_WITH_KNOTS ( 'NONE', 3,
 ( #5315, #3966, #1435, #7621, #12414, #397, #7459, #6437, #14852, #13440, #8795, #8642, #8881, #13672 ),
 .UNSPECIFIED., .F., .F.,
 ( 4, 2, 2, 2, 2, 2, 4 ),
 ( 0.003185368397584303207, 0.003588618066394591230, 0.003991867735204879253, 0.004798367072825484789, 0.005201616741635828323, 0.005604866410446171857, 0.006411365748066773056 ),
 .UNSPECIFIED. ) ;
#9723 = CARTESIAN_POINT ( 'NONE',  ( -224.5735671299499927, 144.8804151761403034, 3.241364612890711427 ) ) ;
#9725 = EDGE_CURVE ( 'NONE', #3061, #10088, #9028, .T. ) ;
#9726 = VERTEX_POINT ( 'NONE', #15233 ) ;
#9727 = CARTESIAN_POINT ( 'NONE',  ( -61.94838851346079167, -181.3058001507315566, -51.45141194869120227 ) ) ;
#9728 = DIRECTION ( 'NONE',  ( -0.000000000000000000, -0.000000000000000000, -1.000000000000000000 ) ) ;
#9729 = AXIS2_PLACEMENT_3D ( 'NONE', #9199, #9040, #3113 ) ;
#9730 = VERTEX_POINT ( 'NONE', #4428 ) ;
#9731 = FACE_OUTER_BOUND ( 'NONE', #9939, .T. ) ;
#9732 = DIRECTION ( 'NONE',  ( -1.000000000000000000, -0.000000000000000000, -0.000000000000000000 ) ) ;
#9733 = TOROIDAL_SURFACE ( 'NONE', #2932, 1.000000000000000000, 0.5000000000000000000 ) ;
#9734 = EDGE_LOOP ( 'NONE', ( #1134, #14535, #13491, #3711 ) ) ;
#9735 = SURFACE_STYLE_FILL_AREA ( #3810 ) ;
#9736 = PLANE ( 'NONE',  #7277 ) ;
#9737 = ORIENTED_EDGE ( 'NONE', *, *, #10291, .F. ) ;
#9738 = CIRCLE ( 'NONE', #8485, 5.000000000000004441 ) ;
#9739 = CARTESIAN_POINT ( 'NONE',  ( 190.5000000000000853, -179.8058001507315566, 52.19066787724494816 ) ) ;
#9740 = DIRECTION ( 'NONE',  ( -0.000000000000000000, -0.000000000000000000, -1.000000000000000000 ) ) ;
#9741 = LINE ( 'NONE', #13432, #2244 ) ;
#9742 = VERTEX_POINT ( 'NONE', #11542 ) ;
#9743 = ORIENTED_EDGE ( 'NONE', *, *, #1633, .F. ) ;
#9744 = CARTESIAN_POINT ( 'NONE',  ( -187.0868153883506011, 133.8486679469899343, -4.640918829492425957 ) ) ;
#9745 = CARTESIAN_POINT ( 'NONE',  ( 204.0369835420791276, 51.66931235154874003, -2.492621690445610216 ) ) ;
#9746 = ORIENTED_EDGE ( 'NONE', *, *, #10848, .T. ) ;
#9747 = DIRECTION ( 'NONE',  ( -0.7071067811864983899, 8.659560562354331352E-17, 0.7071067811865966446 ) ) ;
#9748 = CARTESIAN_POINT ( 'NONE',  ( -144.0627431139473345, 95.36268816863731956, 5.000000000000000000 ) ) ;
#9749 = VECTOR ( 'NONE', #9635, 1000.000000000000000 ) ;
#9750 = DIRECTION ( 'NONE',  ( 0.000000000000000000, 0.000000000000000000, -1.000000000000000000 ) ) ;
#9751 = CIRCLE ( 'NONE', #2944, 59.90987050789675550 ) ;
#9752 = ADVANCED_FACE ( 'NONE', ( #2061, #12642, #14056 ), #10362, .T. ) ;
#9753 = EDGE_LOOP ( 'NONE', ( #2074, #5645, #15466, #10846 ) ) ;
#9754 = ADVANCED_FACE ( 'NONE', ( #11473 ), #11708, .F. ) ;
#9755 = CARTESIAN_POINT ( 'NONE',  ( 198.5423134874356208, 52.64753739496011065, -2.122073255223759780 ) ) ;
#9756 = ORIENTED_EDGE ( 'NONE', *, *, #2025, .F. ) ;
#9757 = LINE ( 'NONE', #7165, #10893 ) ;
#9758 = CARTESIAN_POINT ( 'NONE',  ( -223.1255854116407420, 142.9625047383971719, -1.483432749446032206 ) ) ;
#9759 = CARTESIAN_POINT ( 'NONE',  ( -224.7459018048070050, 144.5716505541534218, -3.023257939496649449 ) ) ;
#9760 = CARTESIAN_POINT ( 'NONE',  ( -76.50000000000001421, 16.03993994372673981, -17.50000000000002487 ) ) ;
#9761 = ORIENTED_EDGE ( 'NONE', *, *, #5421, .F. ) ;
#9762 = CARTESIAN_POINT ( 'NONE',  ( -188.3680287392151627, 131.4989828868489781, 10.16010209732750269 ) ) ;
#9763 = PLANE ( 'NONE',  #12627 ) ;
#9764 = ORIENTED_EDGE ( 'NONE', *, *, #4649, .T. ) ;
#9765 = ORIENTED_EDGE ( 'NONE', *, *, #7417, .F. ) ;
#9766 = DIRECTION ( 'NONE',  ( -1.000000000000000000, 0.000000000000000000, 0.000000000000000000 ) ) ;
#9767 = DIRECTION ( 'NONE',  ( -0.000000000000000000, -0.000000000000000000, -1.000000000000000000 ) ) ;
#9768 = DIRECTION ( 'NONE',  ( -0.000000000000000000, -0.000000000000000000, -1.000000000000000000 ) ) ;
#9769 = FACE_OUTER_BOUND ( 'NONE', #6387, .T. ) ;
#9770 = LINE ( 'NONE', #3848, #14113 ) ;
#9771 = EDGE_CURVE ( 'NONE', #11835, #10665, #7102, .T. ) ;
#9772 = CARTESIAN_POINT ( 'NONE',  ( 68.56535645333921991, 38.79159067395544014, 10.00000000000000178 ) ) ;
#9773 = CARTESIAN_POINT ( 'NONE',  ( -156.6477983077465410, 110.1970436846185066, 0.000000000000000000 ) ) ;
#9774 = CARTESIAN_POINT ( 'NONE',  ( -177.3557003870508595, 132.9282874014947140, 2.500000000000000000 ) ) ;
#9775 = DIRECTION ( 'NONE',  ( 0.000000000000000000, 0.7071067811865474617, 0.7071067811865474617 ) ) ;
#9776 = DIRECTION ( 'NONE',  ( 1.000000000000000000, 0.000000000000000000, 0.000000000000000000 ) ) ;
#9777 = ORIENTED_EDGE ( 'NONE', *, *, #7639, .T. ) ;
#9778 = EDGE_CURVE ( 'NONE', #2210, #2673, #6348, .T. ) ;
#9779 = ORIENTED_EDGE ( 'NONE', *, *, #2025, .T. ) ;
#9780 = CARTESIAN_POINT ( 'NONE',  ( 122.5806775638430253, 45.00321902537314145, 10.00000000000000178 ) ) ;
#9781 = CARTESIAN_POINT ( 'NONE',  ( 64.00000000000005684, 64.53993994372673626, 18.52500000000070202 ) ) ;
#9782 = CIRCLE ( 'NONE', #11043, 1.000000000000000888 ) ;
#9783 = CARTESIAN_POINT ( 'NONE',  ( 70.26535645333922275, 38.79159067395544014, 10.00000000000000178 ) ) ;
#9784 = DIRECTION ( 'NONE',  ( -0.000000000000000000, -0.000000000000000000, -1.000000000000000000 ) ) ;
#9785 = CARTESIAN_POINT ( 'NONE',  ( -34.79899788034579444, 48.72489408690345414, 5.000000000000000000 ) ) ;
#9786 = DIRECTION ( 'NONE',  ( 0.000000000000000000, 0.000000000000000000, -1.000000000000000000 ) ) ;
#9787 = CARTESIAN_POINT ( 'NONE',  ( -179.9311234670130943, 134.3555102485248369, 3.478855109513426580 ) ) ;
#9788 = ORIENTED_EDGE ( 'NONE', *, *, #6508, .T. ) ;
#9789 = ADVANCED_FACE ( 'NONE', ( #7769 ), #8861, .T. ) ;
#9790 = AXIS2_PLACEMENT_3D ( 'NONE', #8456, #9709, #7267 ) ;
#9791 = CIRCLE ( 'NONE', #2987, 0.5000000000000001110 ) ;
#9792 = CIRCLE ( 'NONE', #9041, 5.000000000000017764 ) ;
#9793 = EDGE_LOOP ( 'NONE', ( #12213, #2858, #11954, #4187 ) ) ;
#9794 = DIRECTION ( 'NONE',  ( -0.8731965799097684000, 0.4873681696970817989, 0.000000000000000000 ) ) ;
#9795 = ORIENTED_EDGE ( 'NONE', *, *, #9048, .T. ) ;
#9796 = CARTESIAN_POINT ( 'NONE',  ( -220.7954037378262058, 147.5269295839602535, 9.866320462745882480 ) ) ;
#9797 = ORIENTED_EDGE ( 'NONE', *, *, #12260, .F. ) ;
#9798 = DIRECTION ( 'NONE',  ( -0.000000000000000000, 1.000000000000000000, -0.000000000000000000 ) ) ;
#9799 = CARTESIAN_POINT ( 'NONE',  ( 209.5898355175288543, 48.01761212650198729, -1.192236766262033232 ) ) ;
#9800 = ORIENTED_EDGE ( 'NONE', *, *, #12306, .F. ) ;
#9801 = CIRCLE ( 'NONE', #2992, 1.499999999999994449 ) ;
#9802 = FACE_OUTER_BOUND ( 'NONE', #8636, .T. ) ;
#9803 = LINE ( 'NONE', #14601, #15128 ) ;
#9804 = AXIS2_PLACEMENT_3D ( 'NONE', #12742, #5580, #10388 ) ;
#9805 = EDGE_CURVE ( 'NONE', #2217, #14095, #12380, .T. ) ;
#9806 = AXIS2_PLACEMENT_3D ( 'NONE', #12571, #2889, #486 ) ;
#9807 = DIRECTION ( 'NONE',  ( -0.000000000000000000, 1.000000000000000000, -0.000000000000000000 ) ) ;
#9808 = ORIENTED_EDGE ( 'NONE', *, *, #9434, .T. ) ;
#9810 = EDGE_CURVE ( 'NONE', #12123, #13122, #13180, .T. ) ;
#9809 = EDGE_CURVE ( 'NONE', #6601, #163, #7612, .T. ) ;
#9811 = EDGE_CURVE ( 'NONE', #6520, #8350, #3409, .T. ) ;
#9812 = VERTEX_POINT ( 'NONE', #9492 ) ;
#9813 = DIRECTION ( 'NONE',  ( 0.000000000000000000, 0.000000000000000000, 1.000000000000000000 ) ) ;
#9814 = VECTOR ( 'NONE', #12287, 1000.000000000000000 ) ;
#9815 = CIRCLE ( 'NONE', #9529, 1.000000000000000888 ) ;
#9816 = EDGE_CURVE ( 'NONE', #12412, #8061, #2034, .T. ) ;
#9817 = ORIENTED_EDGE ( 'NONE', *, *, #12839, .T. ) ;
#9818 = DIRECTION ( 'NONE',  ( 1.000000000000000000, 0.000000000000000000, 0.000000000000000000 ) ) ;
#9819 = AXIS2_PLACEMENT_3D ( 'NONE', #13998, #3189, #8019 ) ;
#9820 = DIRECTION ( 'NONE',  ( -0.000000000000000000, 1.000000000000000000, -0.000000000000000000 ) ) ;
#9821 = CARTESIAN_POINT ( 'NONE',  ( -76.50000000000001421, 17.53993994372674692, -17.50000000000002487 ) ) ;
#9822 = ORIENTED_EDGE ( 'NONE', *, *, #5987, .T. ) ;
#9823 = EDGE_LOOP ( 'NONE', ( #13196, #15427 ) ) ;
#9824 = CARTESIAN_POINT ( 'NONE',  ( -208.4264987254875052, 144.6230976266233483, -4.640918829492436615 ) ) ;
#9825 = CARTESIAN_POINT ( 'NONE',  ( 201.2658342953964166, 49.58143373454755931, -3.806719548689701416 ) ) ;
#9826 = VERTEX_POINT ( 'NONE', #14288 ) ;
#9827 = CARTESIAN_POINT ( 'NONE',  ( 5.799999999999999822, 0.000000000000000000, 0.000000000000000000 ) ) ;
#9828 = CARTESIAN_POINT ( 'NONE',  ( -110.0000000000000426, 19.53993994372674337, 9.999999999999998224 ) ) ;
#9829 = AXIS2_PLACEMENT_3D ( 'NONE', #7307, #4764, #2474 ) ;
#9830 = DIRECTION ( 'NONE',  ( -0.8204839007831782327, 0.5707893219124419160, -0.03171306586179808984 ) ) ;
#9831 = VECTOR ( 'NONE', #162, 1000.000000000000114 ) ;
#9832 = AXIS2_PLACEMENT_3D ( 'NONE', #13003, #14114, #14188 ) ;
#9833 = EDGE_CURVE ( 'NONE', #1592, #11107, #3640, .T. ) ;
#9834 = EDGE_CURVE ( 'NONE', #3200, #1354, #10881, .T. ) ;
#9835 = ORIENTED_EDGE ( 'NONE', *, *, #5254, .F. ) ;
#9836 = AXIS2_PLACEMENT_3D ( 'NONE', #5735, #8124, #5811 ) ;
#9837 = CARTESIAN_POINT ( 'NONE',  ( 209.5657782771801578, 33.68426770849990959, -3.244931658323684687 ) ) ;
#9838 = VERTEX_POINT ( 'NONE', #7050 ) ;
#9839 = DIRECTION ( 'NONE',  ( -1.000000000000000000, 0.000000000000000000, 0.000000000000000000 ) ) ;
#9840 = CARTESIAN_POINT ( 'NONE',  ( -217.3067432674630197, 153.8362354792185158, -1.714361214038438552 ) ) ;
#9841 = TOROIDAL_SURFACE ( 'NONE', #14851, 1.000000000000000000, 0.5000000000000000000 ) ;
#9842 = EDGE_CURVE ( 'NONE', #5777, #7205, #10753, .T. ) ;
#9843 = CARTESIAN_POINT ( 'NONE',  ( -179.8633755235878198, 122.3938961877832696, -4.689260562946571120 ) ) ;
#9844 = AXIS2_PLACEMENT_3D ( 'NONE', #4433, #15084, #9267 ) ;
#9845 = DIRECTION ( 'NONE',  ( 0.000000000000000000, -0.9902680687415712502, -0.1391731009600586100 ) ) ;
#9846 = ORIENTED_EDGE ( 'NONE', *, *, #15273, .F. ) ;
#9847 = CARTESIAN_POINT ( 'NONE',  ( -172.0064303153328638, 119.3480080297071595, 9.396848320176498959 ) ) ;
#9848 = VECTOR ( 'NONE', #12490, 1000.000000000000000 ) ;
#9849 = CARTESIAN_POINT ( 'NONE',  ( 205.5810540386909508, 47.77928077683765906, 0.5047415929677595559 ) ) ;
#9850 = ORIENTED_EDGE ( 'NONE', *, *, #6019, .F. ) ;
#9851 = ORIENTED_EDGE ( 'NONE', *, *, #839, .T. ) ;
#9852 = ADVANCED_FACE ( 'NONE', ( #11860 ), #8117, .T. ) ;
#9853 = EDGE_CURVE ( 'NONE', #10500, #10070, #10600, .T. ) ;
#9854 = CARTESIAN_POINT ( 'NONE',  ( 0.1317522424472134801, 1.959574484719845300, 8.000000000000007105 ) ) ;
#9855 = DIRECTION ( 'NONE',  ( 0.000000000000000000, 0.9569673715906176215, 0.2901955370279575286 ) ) ;
#9856 = CIRCLE ( 'NONE', #15118, 3.525000000000000355 ) ;
#9857 = VECTOR ( 'NONE', #14253, 1000.000000000000000 ) ;
#9858 = CARTESIAN_POINT ( 'NONE',  ( -63.50000000000002842, 15.17911304468680100, 9.062306170389884841 ) ) ;
#9859 = CARTESIAN_POINT ( 'NONE',  ( -105.7032403413611092, 68.63699971342413164, 10.00000000000000178 ) ) ;
#9860 = CARTESIAN_POINT ( 'NONE',  ( -207.1387806695930749, 146.9236570583465209, 7.919662025281895446 ) ) ;
#9861 = DIRECTION ( 'NONE',  ( -0.000000000000000000, -0.9902680687415712502, -0.1391731009600586100 ) ) ;
#9862 = VECTOR ( 'NONE', #9495, 1000.000000000000000 ) ;
#9863 = CARTESIAN_POINT ( 'NONE',  ( -110.0000000000000426, 56.53993994372675047, 25.00000000000000000 ) ) ;
#9864 = ORIENTED_EDGE ( 'NONE', *, *, #2684, .T. ) ;
#9866 = AXIS2_PLACEMENT_3D ( 'NONE', #2135, #5698, #14131 ) ;
#9865 = DIRECTION ( 'NONE',  ( -0.7071067811864983899, 8.659560562354331352E-17, 0.7071067811865966446 ) ) ;
#9867 = ORIENTED_EDGE ( 'NONE', *, *, #5187, .F. ) ;
#9868 = CARTESIAN_POINT ( 'NONE',  ( -110.0000000000000426, 22.53993994372673981, 24.99999999999999645 ) ) ;
#9869 = LINE ( 'NONE', #12218, #3085 ) ;
#9870 = SURFACE_STYLE_USAGE ( .BOTH. , #5042 ) ;
#9871 = CARTESIAN_POINT ( 'NONE',  ( 0.000000000000000000, 0.000000000000000000, 0.000000000000000000 ) ) ;
#9872 = CARTESIAN_POINT ( 'NONE',  ( 2.000000000000000000, 3.175426480542944407, 0.000000000000000000 ) ) ;
#9873 = CARTESIAN_POINT ( 'NONE',  ( 184.0000000000000568, -201.3058001507315566, 76.45141194869098911 ) ) ;
#9874 = DIRECTION ( 'NONE',  ( -0.000000000000000000, -0.000000000000000000, -1.000000000000000000 ) ) ;
#9875 = ORIENTED_EDGE ( 'NONE', *, *, #9331, .F. ) ;
#9876 = VECTOR ( 'NONE', #11742, 1000.000000000000000 ) ;
#9877 = LINE ( 'NONE', #14896, #10434 ) ;
#9878 = CLOSED_SHELL ( 'NONE', ( #12502, #3237, #4629, #11536, #9417, #3901, #6960, #13895, #13465, #15349, #8251, #1464, #9398, #10089, #6680, #13784, #8673, #9852, #11435, #10582, #415, #13692, #5636, #13733, #6626, #6665, #12684, #14812, #12757 ) ) ;
#9879 = CARTESIAN_POINT ( 'NONE',  ( 190.0000000000000853, -179.3058001507315566, 64.88378295107887084 ) ) ;
#9880 = CARTESIAN_POINT ( 'NONE',  ( -221.8818932461130942, 149.7029714605600930, 7.941079238973655308 ) ) ;
#9881 = ORIENTED_EDGE ( 'NONE', *, *, #11392, .T. ) ;
#9882 = CARTESIAN_POINT ( 'NONE',  ( -223.5913358527620005, 146.6402366934796078, 9.270357946057281140 ) ) ;
#9883 = EDGE_LOOP ( 'NONE', ( #12907, #12555 ) ) ;
#9884 = CARTESIAN_POINT ( 'NONE',  ( -173.5206377105050990, 117.3432113310319380, -2.605937114841728075 ) ) ;
#9885 = CARTESIAN_POINT ( 'NONE',  ( 198.4352148337827657, 52.62210158206652721, -6.689706441523388669 ) ) ;
#9886 = AXIS2_PLACEMENT_3D ( 'NONE', #3153, #7987, #12773 ) ;
#9887 = ORIENTED_EDGE ( 'NONE', *, *, #13066, .T. ) ;
#9888 = CYLINDRICAL_SURFACE ( 'NONE', #3358, 1.499999999999994227 ) ;
#9889 = DIRECTION ( 'NONE',  ( -0.000000000000000000, 1.000000000000000000, 6.938893903907227145E-17 ) ) ;
#9890 = CONICAL_SURFACE ( 'NONE', #5842, 8.000000000000028422, 1.047197551196600296 ) ;
#9891 = EDGE_CURVE ( 'NONE', #11360, #3344, #1033, .T. ) ;
#9892 = LINE ( 'NONE', #5295, #11170 ) ;
#9893 = ORIENTED_EDGE ( 'NONE', *, *, #4851, .F. ) ;
#9894 = AXIS2_PLACEMENT_3D ( 'NONE', #11128, #7424, #2516 ) ;
#9895 = ORIENTED_EDGE ( 'NONE', *, *, #10969, .F. ) ;
#9896 = CARTESIAN_POINT ( 'NONE',  ( -156.6477983077465410, 110.1970436846185066, 84.88378295107887084 ) ) ;
#9897 = ORIENTED_EDGE ( 'NONE', *, *, #4021, .T. ) ;
#9898 = ADVANCED_FACE ( 'NONE', ( #11781 ), #4741, .T. ) ;
#9899 = DIRECTION ( 'NONE',  ( -0.000000000000000000, -0.000000000000000000, 1.000000000000000000 ) ) ;
#9900 = FACE_OUTER_BOUND ( 'NONE', #10325, .T. ) ;
#9901 = ORIENTED_EDGE ( 'NONE', *, *, #12268, .T. ) ;
#9902 = ORIENTED_EDGE ( 'NONE', *, *, #2443, .T. ) ;
#9903 = CARTESIAN_POINT ( 'NONE',  ( -201.8658614229783268, 146.6084512934502584, 2.500000000000000000 ) ) ;
#9904 = CARTESIAN_POINT ( 'NONE',  ( 163.8799681884088955, 14.47802019457520473, -6.855649852481113804 ) ) ;
#9905 = EDGE_CURVE ( 'NONE', #15478, #8543, #14367, .T. ) ;
#9906 = ORIENTED_EDGE ( 'NONE', *, *, #4337, .F. ) ;
#9907 = FACE_OUTER_BOUND ( 'NONE', #1772, .T. ) ;
#9908 = DIRECTION ( 'NONE',  ( 1.000000000000000000, -2.751328491981765035E-32, 3.965082230804130220E-16 ) ) ;
#9909 = EDGE_CURVE ( 'NONE', #9404, #2275, #11652, .T. ) ;
#9910 = AXIS2_PLACEMENT_3D ( 'NONE', #1580, #6416, #7445 ) ;
#9911 = FACE_OUTER_BOUND ( 'NONE', #729, .T. ) ;
#9912 = CARTESIAN_POINT ( 'NONE',  ( -85.99999999999994316, 64.53993994372673626, 13.30000000000175575 ) ) ;
#9913 = CARTESIAN_POINT ( 'NONE',  ( 201.3430548014149792, 49.57506994421799362, -2.237714600605053228 ) ) ;
#9914 = EDGE_LOOP ( 'NONE', ( #4936, #4248, #10663, #2946 ) ) ;
#9915 = DIRECTION ( 'NONE',  ( -0.000000000000000000, 0.000000000000000000, 1.000000000000000000 ) ) ;
#9916 = CARTESIAN_POINT ( 'NONE',  ( -223.0109838976775620, 143.1868724232609225, -1.877048790282907831 ) ) ;
#9917 = APPLICATION_CONTEXT ( 'automotive_design' ) ;
#9918 = CARTESIAN_POINT ( 'NONE',  ( -218.2851610432379346, 147.7600012847656217, -5.230826428279595319 ) ) ;
#9919 = DIRECTION ( 'NONE',  ( 0.000000000000000000, 0.1391731009600592484, -0.9902680687415712502 ) ) ;
#9920 = ORIENTED_EDGE ( 'NONE', *, *, #625, .T. ) ;
#9921 = CARTESIAN_POINT ( 'NONE',  ( -222.1166800156826184, 149.2823141075699880, 10.12588066961105504 ) ) ;
#9922 = AXIS2_PLACEMENT_3D ( 'NONE', #5613, #7993, #1964 ) ;
#9923 = CARTESIAN_POINT ( 'NONE',  ( 191.3844089520862894, 42.02011290432638901, -3.056456915890917170 ) ) ;
#9924 = EDGE_CURVE ( 'NONE', #14943, #1809, #1109, .T. ) ;
#9925 = EDGE_CURVE ( 'NONE', #4605, #10761, #6855, .T. ) ;
#9926 = EDGE_LOOP ( 'NONE', ( #13499, #8988, #15486, #2983 ) ) ;
#9927 = EDGE_CURVE ( 'NONE', #15218, #4350, #12013, .T. ) ;
#9928 = VERTEX_POINT ( 'NONE', #10836 ) ;
#9929 = CARTESIAN_POINT ( 'NONE',  ( -64.00000000000002842, -179.3058001507315851, 64.88378295107887084 ) ) ;
#9930 = LINE ( 'NONE', #14720, #11768 ) ;
#9931 = CARTESIAN_POINT ( 'NONE',  ( -224.5272311401201648, 144.9634333754441400, 1.130582765288308034 ) ) ;
#9932 = LINE ( 'NONE', #12277, #9432 ) ;
#9933 = FACE_OUTER_BOUND ( 'NONE', #8242, .T. ) ;
#9934 = ADVANCED_FACE ( 'NONE', ( #12083 ), #10516, .F. ) ;
#9935 = AXIS2_PLACEMENT_3D ( 'NONE', #5742, #3300, #12992 ) ;
#9936 = CARTESIAN_POINT ( 'NONE',  ( -199.6024142766798946, 142.8729305612646385, 7.919662025281897222 ) ) ;
#9937 = DIRECTION ( 'NONE',  ( 0.000000000000000000, 0.000000000000000000, -1.000000000000000000 ) ) ;
#9938 = CARTESIAN_POINT ( 'NONE',  ( 190.5000000000000568, 16.03993994372673981, -3.075184203610571654 ) ) ;
#9939 = EDGE_LOOP ( 'NONE', ( #7571, #3481, #2091, #5132 ) ) ;
#9940 = DIRECTION ( 'NONE',  ( 0.000000000000000000, 0.000000000000000000, -1.000000000000000000 ) ) ;
#9941 = ORIENTED_EDGE ( 'NONE', *, *, #10593, .T. ) ;
#9942 = ORIENTED_EDGE ( 'NONE', *, *, #5440, .T. ) ;
#9943 = CARTESIAN_POINT ( 'NONE',  ( -150.5358285740960014, 107.7783824288041217, 9.802099390037296800 ) ) ;
#9944 = CARTESIAN_POINT ( 'NONE',  ( -35.99999999999995026, 64.53993994372673626, 18.52500000000140190 ) ) ;
#9945 = FACE_OUTER_BOUND ( 'NONE', #2613, .T. ) ;
#9946 = PLANE ( 'NONE',  #14197 ) ;
#9947 = CARTESIAN_POINT ( 'NONE',  ( -76.50000000000001421, 19.53993994372674692, -17.50000000000002487 ) ) ;
#9948 = LINE ( 'NONE', #1476, #7072 ) ;
#9949 = CARTESIAN_POINT ( 'NONE',  ( -169.9361637590235716, 128.7768979049109532, 3.478855110294483133 ) ) ;
#9950 = AXIS2_PLACEMENT_3D ( 'NONE', #4875, #109, #2658 ) ;
#9951 = ORIENTED_EDGE ( 'NONE', *, *, #2540, .F. ) ;
#9952 = EDGE_CURVE ( 'NONE', #101, #227, #947, .T. ) ;
#9953 = LINE ( 'NONE', #5205, #14946 ) ;
#9954 = EDGE_CURVE ( 'NONE', #10673, #3263, #3827, .T. ) ;
#9955 = PRODUCT_DEFINITION_CONTEXT ( 'detailed design', #15611, 'design' ) ;
#9956 = EDGE_CURVE ( 'NONE', #9422, #13622, #10035, .T. ) ;
#9957 = CIRCLE ( 'NONE', #4642, 0.9999999999999991118 ) ;
#9958 = CARTESIAN_POINT ( 'NONE',  ( 193.1249951165660548, 46.22013307728793308, -3.310989833511668756 ) ) ;
#9959 = CARTESIAN_POINT ( 'NONE',  ( -76.00000000000001421, 15.10952649420676863, 9.557440204760682789 ) ) ;
#9960 = VERTEX_POINT ( 'NONE', #1338 ) ;
#9961 = CARTESIAN_POINT ( 'NONE',  ( -220.9030130636566298, 151.4567889657070339, 9.535387874750053783 ) ) ;
#9962 = EDGE_LOOP ( 'NONE', ( #9651, #2974, #14365, #15493 ) ) ;
#9963 = CARTESIAN_POINT ( 'NONE',  ( -167.8857020579134200, 127.4390830883378953, 0.6628302033481980882 ) ) ;
#9964 = FACE_OUTER_BOUND ( 'NONE', #4504, .T. ) ;
#9965 = ORIENTED_EDGE ( 'NONE', *, *, #6762, .F. ) ;
#9966 = CARTESIAN_POINT ( 'NONE',  ( 215.1062858801516882, 25.86394065090268057, 18.00000000000000355 ) ) ;
#9967 = FACE_OUTER_BOUND ( 'NONE', #4681, .T. ) ;
#9968 = AXIS2_PLACEMENT_3D ( 'NONE', #819, #13861, #13940 ) ;
#9969 = EDGE_CURVE ( 'NONE', #1126, #3245, #2615, .T. ) ;
#9970 = CARTESIAN_POINT ( 'NONE',  ( -64.00000000000002842, -178.6666270497714777, 53.18093594598651919 ) ) ;
#9971 = ORIENTED_EDGE ( 'NONE', *, *, #3662, .T. ) ;
#9972 = ADVANCED_FACE ( 'NONE', ( #9964 ), #1547, .T. ) ;
#9973 = DIRECTION ( 'NONE',  ( 1.156482317317871725E-16, -1.156482317317871725E-16, 1.000000000000000000 ) ) ;
#9974 = ORIENTED_EDGE ( 'NONE', *, *, #4894, .T. ) ;
#9975 = DIRECTION ( 'NONE',  ( -1.000000000000000000, -6.938893903907222067E-15, 0.000000000000000000 ) ) ;
#9976 = FACE_OUTER_BOUND ( 'NONE', #7241, .T. ) ;
#9977 = VERTEX_POINT ( 'NONE', #8769 ) ;
#9978 = CARTESIAN_POINT ( 'NONE',  ( -70.00000000000000000, 17.53993994372673981, -10.99999999999999645 ) ) ;
#9979 = CIRCLE ( 'NONE', #3661, 0.5000000000000004441 ) ;
#9980 = DIRECTION ( 'NONE',  ( -1.000000000000000000, 0.000000000000000000, -0.000000000000000000 ) ) ;
#9981 = ORIENTED_EDGE ( 'NONE', *, *, #2082, .T. ) ;
#9982 = ORIENTED_EDGE ( 'NONE', *, *, #8786, .T. ) ;
#9983 = CARTESIAN_POINT ( 'NONE',  ( -198.5677679834141713, 144.7676449960911498, 2.500000000000000000 ) ) ;
#9984 = EDGE_CURVE ( 'NONE', #8651, #5373, #15542, .T. ) ;
#9985 = CARTESIAN_POINT ( 'NONE',  ( 208.8186272397570349, 39.68461847005694665, -7.558035125831273682 ) ) ;
#9986 = VERTEX_POINT ( 'NONE', #6411 ) ;
#9987 = CYLINDRICAL_SURFACE ( 'NONE', #13593, 3.500000000000003109 ) ;
#9988 = DIRECTION ( 'NONE',  ( 0.5000000000000000000, -0.8660254037844385966, 0.000000000000000000 ) ) ;
#9989 = DIRECTION ( 'NONE',  ( -0.000000000000000000, -0.000000000000000000, -1.000000000000000000 ) ) ;
#9990 = CIRCLE ( 'NONE', #11493, 1.500000000000000000 ) ;
#9991 = APPLICATION_CONTEXT ( 'automotive_design' ) ;
#9992 = ADVANCED_FACE ( 'NONE', ( #372 ), #6795, .F. ) ;
#9993 = DIRECTION ( 'NONE',  ( 0.000000000000000000, 0.1391731009600592484, -0.9902680687415712502 ) ) ;
#9994 = CARTESIAN_POINT ( 'NONE',  ( 205.3727474927790411, 33.82195144205066839, -0.3638485434072702973 ) ) ;
#9995 = ORIENTED_EDGE ( 'NONE', *, *, #5171, .F. ) ;
#9996 = LINE ( 'NONE', #13761, #2304 ) ;
#9997 = CARTESIAN_POINT ( 'NONE',  ( -221.8246199127426053, 145.4969522655044329, -4.202312765555400453 ) ) ;
#9998 = CARTESIAN_POINT ( 'NONE',  ( -184.7739606708014719, 119.6463200498024548, -0.4555467707853387282 ) ) ;
#9999 = CARTESIAN_POINT ( 'NONE',  ( 178.0000000000000853, 15.03993994372673804, 38.07518420361041933 ) ) ;
#10000 = ORIENTED_EDGE ( 'NONE', *, *, #9771, .T. ) ;
#10001 = CARTESIAN_POINT ( 'NONE',  ( -181.0973828845548610, 120.1829782941312743, 7.859965607560862821 ) ) ;
#10002 = CARTESIAN_POINT ( 'NONE',  ( 201.3402840685550643, 32.17245832385849980, -2.180909807981465054 ) ) ;
#10003 = ORIENTED_EDGE ( 'NONE', *, *, #392, .T. ) ;
#10004 = ORIENTED_EDGE ( 'NONE', *, *, #3664, .T. ) ;
#10005 = TOROIDAL_SURFACE ( 'NONE', #5711, 6.999999999999991118, 2.000000000000000000 ) ;
#10006 = CARTESIAN_POINT ( 'NONE',  ( 3.233971792616918695E-15, -6.534749472788175417, -4.681481898396977925 ) ) ;
#10007 = DIRECTION ( 'NONE',  ( 0.000000000000000000, 0.000000000000000000, 1.000000000000000000 ) ) ;
#10008 = DIRECTION ( 'NONE',  ( 1.000000000000000000, 0.000000000000000000, -0.000000000000000000 ) ) ;
#10009 = ADVANCED_FACE ( 'NONE', ( #15138 ), #12465, .F. ) ;
#10010 = DIRECTION ( 'NONE',  ( 0.000000000000000000, 0.5000000000000012212, 0.8660254037844380415 ) ) ;
#10012 = ADVANCED_FACE ( 'NONE', ( #5451 ), #11288, .F. ) ;
#10011 = EDGE_CURVE ( 'NONE', #10092, #5037, #1654, .T. ) ;
#10013 = VECTOR ( 'NONE', #8459, 1000.000000000000000 ) ;
#10014 = CARTESIAN_POINT ( 'NONE',  ( 0.000000000000000000, 0.000000000000000000, 0.000000000000000000 ) ) ;
#10015 = FACE_OUTER_BOUND ( 'NONE', #7147, .T. ) ;
#10016 = CARTESIAN_POINT ( 'NONE',  ( -34.79899788034579444, 48.72489408690345414, 0.000000000000000000 ) ) ;
#10017 = ORIENTED_EDGE ( 'NONE', *, *, #15336, .T. ) ;
#10018 = DIRECTION ( 'NONE',  ( 1.000000000000000000, 1.669238443041287922E-16, 0.000000000000000000 ) ) ;
#10019 = VERTEX_POINT ( 'NONE', #449 ) ;
#10020 = EDGE_LOOP ( 'NONE', ( #11929, #1009, #4511, #6911 ) ) ;
#10021 = LINE ( 'NONE', #13873, #9814 ) ;
#10022 = CARTESIAN_POINT ( 'NONE',  ( 190.5000000000000568, -178.8753867012115961, 64.82329228561619061 ) ) ;
#10023 = CARTESIAN_POINT ( 'NONE',  ( 164.0000000000000568, 62.13993994372673768, 11.50000000000000000 ) ) ;
#10024 = DIRECTION ( 'NONE',  ( -0.000000000000000000, 1.000000000000000000, -0.000000000000000000 ) ) ;
#10025 = CARTESIAN_POINT ( 'NONE',  ( -219.4693564981101588, 154.0254097489945764, 1.294062626199961930 ) ) ;
#10026 = CARTESIAN_POINT ( 'NONE',  ( -172.3625742532922800, 130.1311808564658747, 3.478855110039204224 ) ) ;
#10027 = EDGE_LOOP ( 'NONE', ( #14135, #14406, #12655 ) ) ;
#10028 = DIRECTION ( 'NONE',  ( -0.000000000000000000, 1.000000000000000000, -0.000000000000000000 ) ) ;
#10029 = DIRECTION ( 'NONE',  ( -0.000000000000000000, 0.000000000000000000, -1.000000000000000000 ) ) ;
#10030 = DIRECTION ( 'NONE',  ( 0.000000000000000000, 1.000000000000000000, 0.000000000000000000 ) ) ;
#10031 = ORIENTED_EDGE ( 'NONE', *, *, #1542, .F. ) ;
#10032 = CARTESIAN_POINT ( 'NONE',  ( -221.8843987189232507, 149.6984825127276224, 7.941366815851232275 ) ) ;
#10033 = ORIENTED_EDGE ( 'NONE', *, *, #4815, .F. ) ;
#10034 = CARTESIAN_POINT ( 'NONE',  ( -170.8583098116105248, 122.1131896768847298, -5.150070920892065196 ) ) ;
#10035 = LINE ( 'NONE', #2693, #29 ) ;
#10036 = VERTEX_POINT ( 'NONE', #4247 ) ;
#10037 = DIRECTION ( 'NONE',  ( -1.000000000000000000, 0.000000000000000000, -0.000000000000000000 ) ) ;
#10038 = CARTESIAN_POINT ( 'NONE',  ( -35.99999999999995026, 62.13993994372673768, 15.00000000000139977 ) ) ;
#10039 = EDGE_CURVE ( 'NONE', #8632, #8731, #14980, .T. ) ;
#10040 = CARTESIAN_POINT ( 'NONE',  ( 190.5000000000000568, 15.53993994372673981, 10.05257423913146475 ) ) ;
#10041 = ORIENTED_EDGE ( 'NONE', *, *, #3994, .T. ) ;
#10042 = CIRCLE ( 'NONE', #9033, 0.5000000000000004441 ) ;
#10043 = APPLICATION_PROTOCOL_DEFINITION ( 'draft international standard', 'automotive_design', 1998, #10793 ) ;
#10044 = ORIENTED_EDGE ( 'NONE', *, *, #9119, .F. ) ;
#10045 = DIRECTION ( 'NONE',  ( -0.000000000000000000, 1.000000000000000000, 8.673617379884035472E-17 ) ) ;
#10046 = CYLINDRICAL_SURFACE ( 'NONE', #15296, 3.500000000000003109 ) ;
#10047 = ORIENTED_EDGE ( 'NONE', *, *, #4211, .T. ) ;
#10048 = AXIS2_PLACEMENT_3D ( 'NONE', #8790, #3962, #2711 ) ;
#10049 = LINE ( 'NONE', #313, #8320 ) ;
#10050 = ORIENTED_EDGE ( 'NONE', *, *, #11037, .T. ) ;
#10051 = ORIENTED_EDGE ( 'NONE', *, *, #1897, .F. ) ;
#10052 = CARTESIAN_POINT ( 'NONE',  ( -64.00000000000002842, 15.53993994372673626, 52.49999999999997868 ) ) ;
#10053 = LINE ( 'NONE', #4041, #11378 ) ;
#10054 = CIRCLE ( 'NONE', #15565, 0.5000000000000004441 ) ;
#10055 = ORIENTED_EDGE ( 'NONE', *, *, #6451, .F. ) ;
#10056 = CARTESIAN_POINT ( 'NONE',  ( 203.2140370934807834, 48.77700970988914264, -0.9247215889056725757 ) ) ;
#10057 = FACE_BOUND ( 'NONE', #8767, .T. ) ;
#10058 = EDGE_CURVE ( 'NONE', #7982, #9410, #9241, .T. ) ;
#10059 = CYLINDRICAL_SURFACE ( 'NONE', #6038, 0.5000000000000004441 ) ;
#10060 = PLANE ( 'NONE',  #14255 ) ;
#10061 = CARTESIAN_POINT ( 'NONE',  ( 163.3793289068652257, 15.80605437029538507, -6.370175303308196924 ) ) ;
#10062 = CIRCLE ( 'NONE', #14336, 1.699999999999993072 ) ;
#10063 = CIRCLE ( 'NONE', #3250, 0.5000000000000004441 ) ;
#10064 = AXIS2_PLACEMENT_3D ( 'NONE', #1532, #10950, #6209 ) ;
#10065 = ORIENTED_EDGE ( 'NONE', *, *, #5334, .T. ) ;
#10066 = FACE_BOUND ( 'NONE', #6000, .T. ) ;
#10067 = DIRECTION ( 'NONE',  ( 0.000000000000000000, 0.000000000000000000, 1.000000000000000000 ) ) ;
#10068 = CARTESIAN_POINT ( 'NONE',  ( -170.7063108826370694, 121.6823135672476752, -5.361935827173478941 ) ) ;
#10069 = LINE ( 'NONE', #6525, #5012 ) ;
#10070 = VERTEX_POINT ( 'NONE', #532 ) ;
#10071 = CARTESIAN_POINT ( 'NONE',  ( -182.0950013669840359, 118.3955881831737997, 1.446957622915671537 ) ) ;
#10072 = CARTESIAN_POINT ( 'NONE',  ( 205.5168546899054434, 47.82311440310952833, -1.064259200291542529 ) ) ;
#10073 = ORIENTED_EDGE ( 'NONE', *, *, #7443, .F. ) ;
#10074 = AXIS2_PLACEMENT_3D ( 'NONE', #3898, #1679, #7537 ) ;
#10075 = CIRCLE ( 'NONE', #13837, 1.000000000000000000 ) ;
#10076 = EDGE_CURVE ( 'NONE', #9198, #13912, #2823, .T. ) ;
#10077 = DIRECTION ( 'NONE',  ( -0.000000000000000000, 0.000000000000000000, 1.000000000000000000 ) ) ;
#10078 = DIRECTION ( 'NONE',  ( -0.1562424607007877608, 0.2866315678550999668, -0.9452145987991775744 ) ) ;
#10079 = AXIS2_PLACEMENT_3D ( 'NONE', #6673, #5478, #1832 ) ;
#10080 = AXIS2_PLACEMENT_3D ( 'NONE', #4235, #14809, #9073 ) ;
#10081 = DIRECTION ( 'NONE',  ( 0.000000000000000000, 0.000000000000000000, 1.000000000000000000 ) ) ;
#10082 = ORIENTED_EDGE ( 'NONE', *, *, #13862, .F. ) ;
#10083 = CIRCLE ( 'NONE', #740, 1.499999999999997780 ) ;
#10084 = CARTESIAN_POINT ( 'NONE',  ( 172.5293059057019889, 61.25683321636181233, 10.00000000000000178 ) ) ;
#10085 = CARTESIAN_POINT ( 'NONE',  ( -167.5097532647548633, 127.4226149533560175, 3.478855110549762042 ) ) ;
#10086 = CARTESIAN_POINT ( 'NONE',  ( 177.5000000000000853, 14.90076684276667862, 37.08491613486885541 ) ) ;
#10087 = DIRECTION ( 'NONE',  ( 0.000000000000000000, 0.000000000000000000, 1.000000000000000000 ) ) ;
#10088 = VERTEX_POINT ( 'NONE', #12623 ) ;
#10089 = ADVANCED_FACE ( 'NONE', ( #6570 ), #8934, .T. ) ;
#10090 = CARTESIAN_POINT ( 'NONE',  ( -163.5368496159778147, 108.5568550452353378, 5.000000000000000000 ) ) ;
#10091 = VERTEX_POINT ( 'NONE', #3084 ) ;
#10092 = VERTEX_POINT ( 'NONE', #10420 ) ;
#10093 = CIRCLE ( 'NONE', #233, 3.524999999999998579 ) ;
#10094 = DIRECTION ( 'NONE',  ( -1.000000000000000000, -4.585547486636276518E-32, 3.965082230804130220E-16 ) ) ;
#10095 = CARTESIAN_POINT ( 'NONE',  ( 178.0000000000000853, 15.53993994372673804, 38.07518420361041933 ) ) ;
#10096 = CIRCLE ( 'NONE', #3282, 380.9270036976043343 ) ;
#10097 = CARTESIAN_POINT ( 'NONE',  ( 164.0000000000000568, 62.13993994372673768, 15.00000000000000355 ) ) ;
#10098 = DIRECTION ( 'NONE',  ( 1.000000000000000000, -0.000000000000000000, -0.000000000000000000 ) ) ;
#10099 = PRODUCT_RELATED_PRODUCT_CATEGORY ( 'part', '', ( #12937 ) ) ;
#10100 = CARTESIAN_POINT ( 'NONE',  ( -217.1902381962481172, 154.0393758339013743, -1.351620443338561017 ) ) ;
#10101 = EDGE_CURVE ( 'NONE', #12639, #7344, #4318, .T. ) ;
#10102 = ORIENTED_EDGE ( 'NONE', *, *, #4971, .F. ) ;
#10103 = AXIS2_PLACEMENT_3D ( 'NONE', #4986, #145, #14524 ) ;
#10104 = CARTESIAN_POINT ( 'NONE',  ( 21.99999999999999289, 0.000000000000000000, 0.000000000000000000 ) ) ;
#10105 = VECTOR ( 'NONE', #9865, 1000.000000000000000 ) ;
#10106 = AXIS2_PLACEMENT_3D ( 'NONE', #4295, #5651, #11657 ) ;
#10107 = CARTESIAN_POINT ( 'NONE',  ( 207.1288103955774318, 46.12660085639766550, -4.186765234109192768 ) ) ;
#10108 = CARTESIAN_POINT ( 'NONE',  ( -157.8787660911425803, 118.6941998492684149, 5.000000000000000000 ) ) ;
#10109 = ORIENTED_EDGE ( 'NONE', *, *, #13862, .T. ) ;
#10110 = CARTESIAN_POINT ( 'NONE',  ( -219.9563263261640316, 153.1529268606066125, 8.541693648944034933 ) ) ;
#10111 = ORIENTED_EDGE ( 'NONE', *, *, #1114, .T. ) ;
#10112 = CARTESIAN_POINT ( 'NONE',  ( -171.0834245745559485, 121.7098612420110442, -5.167027133578317333 ) ) ;
#10113 = DIRECTION ( 'NONE',  ( 1.669238443041287429E-16, -1.000000000000000000, 0.000000000000000000 ) ) ;
#10114 = EDGE_CURVE ( 'NONE', #3245, #12123, #13728, .T. ) ;
#10115 = EDGE_LOOP ( 'NONE', ( #7281, #7920 ) ) ;
#10116 = ADVANCED_FACE ( 'NONE', ( #686 ), #15152, .T. ) ;
#10117 = PLANE ( 'NONE',  #4383 ) ;
#10118 = CARTESIAN_POINT ( 'NONE',  ( 190.5000000000000568, 15.03993994372673981, -3.075184203610571654 ) ) ;
#10119 = AXIS2_PLACEMENT_3D ( 'NONE', #7567, #12366, #348 ) ;
#10120 = AXIS2_PLACEMENT_3D ( 'NONE', #10790, #8508, #9452 ) ;
#10121 = DIRECTION ( 'NONE',  ( 0.000000000000000000, 0.000000000000000000, -1.000000000000000000 ) ) ;
#10122 = ORIENTED_EDGE ( 'NONE', *, *, #9810, .T. ) ;
#10123 = CONTEXT_DEPENDENT_SHAPE_REPRESENTATION ( #14507, #5377 ) ;
#10124 = VERTEX_POINT ( 'NONE', #7912 ) ;
#10125 = CARTESIAN_POINT ( 'NONE',  ( 17.41029453487719181, 40.04259805664093363, 7.600000000000002309 ) ) ;
#10126 = ORIENTED_EDGE ( 'NONE', *, *, #10920, .T. ) ;
#10127 = CARTESIAN_POINT ( 'NONE',  ( -70.00000000000000000, 17.53993994372673981, -12.49999999999999289 ) ) ;
#10128 = CIRCLE ( 'NONE', #521, 1.699999999999991518 ) ;
#10129 = EDGE_CURVE ( 'NONE', #8453, #1214, #784, .T. ) ;
#10130 = CARTESIAN_POINT ( 'NONE',  ( 190.0000000000000568, -179.3058001507315566, -17.76585208085566947 ) ) ;
#10131 = ORIENTED_EDGE ( 'NONE', *, *, #2880, .T. ) ;
#10132 = ORIENTED_EDGE ( 'NONE', *, *, #2545, .F. ) ;
#10133 = CIRCLE ( 'NONE', #11886, 0.5000000000000004441 ) ;
#10134 = CARTESIAN_POINT ( 'NONE',  ( -167.5053995445195767, 127.4304153265770907, 2.500000001036336350 ) ) ;
#10135 = DIRECTION ( 'NONE',  ( -0.000000000000000000, -0.000000000000000000, 1.000000000000000000 ) ) ;
#10136 = ORIENTED_EDGE ( 'NONE', *, *, #4399, .T. ) ;
#10137 = DIRECTION ( 'NONE',  ( 0.000000000000000000, 0.000000000000000000, 1.000000000000000000 ) ) ;
#10138 = CARTESIAN_POINT ( 'NONE',  ( 166.3583383998781358, 57.46267437295986014, 5.000000000000000000 ) ) ;
#10139 = CARTESIAN_POINT ( 'NONE',  ( -63.50000000000002842, 15.47035339324670922, 37.00486596562913633 ) ) ;
#10140 = CARTESIAN_POINT ( 'NONE',  ( 178.0000000000000853, -178.8058001507315566, -17.19066787724516843 ) ) ;
#10141 = DIRECTION ( 'NONE',  ( 0.000000000000000000, 0.000000000000000000, -1.000000000000000000 ) ) ;
#10142 = VECTOR ( 'NONE', #12460, 1000.000000000000000 ) ;
#10143 = CARTESIAN_POINT ( 'NONE',  ( 190.5000000000000853, -179.8058001507315566, 52.76585208085545275 ) ) ;
#10144 = ADVANCED_FACE ( 'NONE', ( #12695, #4330 ), #11373, .F. ) ;
#10145 = EDGE_LOOP ( 'NONE', ( #2129, #4137, #3719, #12949 ) ) ;
#10146 =( LENGTH_UNIT ( ) NAMED_UNIT ( * ) SI_UNIT ( .MILLI., .METRE. ) );
#10147 = DIRECTION ( 'NONE',  ( -0.000000000000000000, -0.000000000000000000, 1.000000000000000000 ) ) ;
#10148 = CARTESIAN_POINT ( 'NONE',  ( -192.3464331062453709, 140.8629472311621100, -0.4547266291960749829 ) ) ;
#10149 = CARTESIAN_POINT ( 'NONE',  ( -223.5918188539070002, 142.0538562971642307, 1.612306317632525854 ) ) ;
#10150 = ORIENTED_EDGE ( 'NONE', *, *, #10794, .T. ) ;
#10151 = CARTESIAN_POINT ( 'NONE',  ( -187.5349220100912930, 120.9938564418671518, 1.515400478619096658 ) ) ;
#10153 = CARTESIAN_POINT ( 'NONE',  ( 202.3171501287270644, 32.63561614260228794, -6.547335233887139339 ) ) ;
#10152 = COLOUR_RGB ( '', 0.31764706, 0.68627451, 0.89019608) ;
#10154 = ORIENTED_EDGE ( 'NONE', *, *, #2424, .F. ) ;
#10155 = LINE ( 'NONE', #9929, #13455 ) ;
#10156 = CARTESIAN_POINT ( 'NONE',  ( 177.5000000000000853, -179.3058001507315566, -17.19066787724516843 ) ) ;
#10157 = CARTESIAN_POINT ( 'NONE',  ( 170.6931741512129577, -3.595212766542494887, -13.46247879130521952 ) ) ;
#10158 = ADVANCED_FACE ( 'NONE', ( #9170 ), #13969, .T. ) ;
#10159 = CARTESIAN_POINT ( 'NONE',  ( 165.1224552381025887, 111.1124422548786299, 0.000000000000000000 ) ) ;
#10160 = VECTOR ( 'NONE', #9497, 1000.000000000000000 ) ;
#10161 = ORIENTED_EDGE ( 'NONE', *, *, #1097, .F. ) ;
#10162 = CARTESIAN_POINT ( 'NONE',  ( 185.1062858801516882, 25.86394065090268057, 18.00000000000000355 ) ) ;
#10163 = CARTESIAN_POINT ( 'NONE',  ( -212.2525635541804547, 150.1126023820536375, 7.919662025281898998 ) ) ;
#10164 = CARTESIAN_POINT ( 'NONE',  ( 190.0000000000000853, -178.8753867012115961, 64.82329228561619061 ) ) ;
#10165 = FACE_OUTER_BOUND ( 'NONE', #6548, .T. ) ;
#10166 = PRODUCT_DEFINITION_SHAPE ( 'NONE', 'NONE',  #15619 ) ;
#10167 = EDGE_LOOP ( 'NONE', ( #7238, #293 ) ) ;
#10168 = TOROIDAL_SURFACE ( 'NONE', #14935, 1.000000000000000000, 0.5000000000000000000 ) ;
#10169 = CARTESIAN_POINT ( 'NONE',  ( 184.0000000000000568, 19.53993994372673626, 47.49999999999997868 ) ) ;
#10170 = ORIENTED_EDGE ( 'NONE', *, *, #3106, .T. ) ;
#10171 = ORIENTED_EDGE ( 'NONE', *, *, #9613, .F. ) ;
#10172 = CYLINDRICAL_SURFACE ( 'NONE', #10822, 0.5000000000000004441 ) ;
#10173 = DIRECTION ( 'NONE',  ( 8.659560562355533132E-17, 0.7071067811864985009, -0.7071067811865965336 ) ) ;
#10174 = ADVANCED_FACE ( 'NONE', ( #1957 ), #8126, .T. ) ;
#10175 = FACE_BOUND ( 'NONE', #8091, .T. ) ;
#10176 = CARTESIAN_POINT ( 'NONE',  ( -216.8935220752126440, 154.5526377852563940, -0.02875724444948107861 ) ) ;
#10177 = CIRCLE ( 'NONE', #1585, 4.999999999999990230 ) ;
#10178 = CARTESIAN_POINT ( 'NONE',  ( -172.2924035267946294, 113.3882749373523922, 0.000000000000000000 ) ) ;
#10179 = ORIENTED_EDGE ( 'NONE', *, *, #7528, .F. ) ;
#10180 = PLANE ( 'NONE',  #3124 ) ;
#10181 = EDGE_CURVE ( 'NONE', #6887, #14401, #3072, .T. ) ;
#10182 = CARTESIAN_POINT ( 'NONE',  ( 203.2140370934807834, 48.77700970988914264, -0.9247215889056725757 ) ) ;
#10183 = CARTESIAN_POINT ( 'NONE',  ( -220.4428784760894473, 152.2811923082724661, -1.958540667262526958 ) ) ;
#10184 = VERTEX_POINT ( 'NONE', #2280 ) ;
#10185 = ADVANCED_BREP_SHAPE_REPRESENTATION ( '', ( #10760, #12337 ), #4745 ) ;
#10186 = CIRCLE ( 'NONE', #6674, 0.5000000000000004441 ) ;
#10187 = CARTESIAN_POINT ( 'NONE',  ( -217.6921401408168322, 153.1680562725702828, 7.596881196942645964 ) ) ;
#10188 = ORIENTED_EDGE ( 'NONE', *, *, #12399, .T. ) ;
#10189 = CARTESIAN_POINT ( 'NONE',  ( -171.1959741278963349, 121.5082110499024139, -5.161946524584423379 ) ) ;
#10190 = CARTESIAN_POINT ( 'NONE',  ( -84.29999999999994031, 62.13993994372673768, 15.00000000000174794 ) ) ;
#10192 = EDGE_LOOP ( 'NONE', ( #105, #4009, #11705 ) ) ;
#10191 = CIRCLE ( 'NONE', #9436, 0.5000000000000004441 ) ;
#10193 = APPLICATION_CONTEXT ( 'automotive_design' ) ;
#10194 = CARTESIAN_POINT ( 'NONE',  ( -64.00000000000002842, -178.8058001507315566, 52.19066787724494816 ) ) ;
#10195 = CARTESIAN_POINT ( 'NONE',  ( 5.799999999999999822, 0.000000000000000000, 0.000000000000000000 ) ) ;
#10196 = CARTESIAN_POINT ( 'NONE',  ( 164.0000000000000568, 62.13993994372673768, 18.50000000000000711 ) ) ;
#10197 = VERTEX_POINT ( 'NONE', #8065 ) ;
#10198 = AXIS2_PLACEMENT_3D ( 'NONE', #13072, #2351, #3538 ) ;
#10199 = B_SPLINE_CURVE_WITH_KNOTS ( 'NONE', 3,
 ( #7338, #7100, #13148, #9463, #4798, #14262 ),
 .UNSPECIFIED., .F., .F.,
 ( 4, 2, 4 ),
 ( 0.02753256082175535926, 0.02987018134127081975, 0.03220780186078627677 ),
 .UNSPECIFIED. ) ;
#10200 = PRODUCT_CONTEXT ( 'NONE', #5939, 'mechanical' ) ;
#10201 = VERTEX_POINT ( 'NONE', #6955 ) ;
#10202 = AXIS2_PLACEMENT_3D ( 'NONE', #1341, #2776, #12085 ) ;
#10203 = EDGE_CURVE ( 'NONE', #8453, #1809, #3391, .T. ) ;
#10204 = EDGE_CURVE ( 'NONE', #13381, #3064, #6552, .T. ) ;
#10205 = CARTESIAN_POINT ( 'NONE',  ( -155.7750080535546147, 110.7025914469866308, 9.802099390037289695 ) ) ;
#10206 = ORIENTED_EDGE ( 'NONE', *, *, #13336, .F. ) ;
#10207 = FACE_BOUND ( 'NONE', #14659, .T. ) ;
#10208 = CARTESIAN_POINT ( 'NONE',  ( 0.2456200930618607225, -3.175426480542939967, 2.004439700231694701E-16 ) ) ;
#10209 = ORIENTED_EDGE ( 'NONE', *, *, #11823, .T. ) ;
#10210 = ORIENTED_EDGE ( 'NONE', *, *, #4340, .T. ) ;
#10211 = CYLINDRICAL_SURFACE ( 'NONE', #4237, 1.700000000000007061 ) ;
#10212 = CARTESIAN_POINT ( 'NONE',  ( 184.0000000000000568, 17.53993994372673626, 47.49999999999997868 ) ) ;
#10213 = AXIS2_PLACEMENT_3D ( 'NONE', #1781, #10316, #12824 ) ;
#10214 = ORIENTED_EDGE ( 'NONE', *, *, #5818, .T. ) ;
#10215 = CARTESIAN_POINT ( 'NONE',  ( 191.4227524587821279, 39.61567282607229856, -2.929995994935606252 ) ) ;
#10216 = DIRECTION ( 'NONE',  ( -0.000000000000000000, -0.000000000000000000, -1.000000000000000000 ) ) ;
#10217 = CARTESIAN_POINT ( 'NONE',  ( 165.7000000000000739, 62.13993994372673768, 15.00000000000000355 ) ) ;
#10218 = CARTESIAN_POINT ( 'NONE',  ( 177.5000000000000853, -179.3058001507315566, 65.31842631998698323 ) ) ;
#10219 = CARTESIAN_POINT ( 'NONE',  ( 5.799999999999999822, 0.000000000000000000, 0.000000000000000000 ) ) ;
#10220 = VECTOR ( 'NONE', #4364, 1000.000000000000000 ) ;
#10221 = CARTESIAN_POINT ( 'NONE',  ( 178.0000000000000853, 16.03993994372673981, 7.553451883674125344E-16 ) ) ;
#10222 = EDGE_LOOP ( 'NONE', ( #9605, #9011, #10389, #1170 ) ) ;
#10223 = PLANE ( 'NONE',  #14238 ) ;
#10224 = CARTESIAN_POINT ( 'NONE',  ( -207.1016862382755335, 146.9901175548950505, -2.963320117457100888 ) ) ;
#10225 = LINE ( 'NONE', #13604, #454 ) ;
#10226 = ORIENTED_EDGE ( 'NONE', *, *, #6962, .T. ) ;
#10227 = CARTESIAN_POINT ( 'NONE',  ( -187.3366327499677197, 121.3409432500951937, 5.434137442415932107 ) ) ;
#10228 = CARTESIAN_POINT ( 'NONE',  ( 188.3492591927541753, 42.47468418338397811, -7.638025320682917396 ) ) ;
#10229 = ORIENTED_EDGE ( 'NONE', *, *, #11167, .T. ) ;
#10230 = VECTOR ( 'NONE', #6585, 1000.000000000000000 ) ;
#10231 = FACE_OUTER_BOUND ( 'NONE', #5582, .T. ) ;
#10232 = DIRECTION ( 'NONE',  ( -1.000000000000000000, -0.000000000000000000, -0.000000000000000000 ) ) ;
#10233 = CIRCLE ( 'NONE', #6467, 1.000000000000000888 ) ;
#10234 = LINE ( 'NONE', #3051, #2026 ) ;
#10235 = EDGE_CURVE ( 'NONE', #13797, #9039, #11762, .T. ) ;
#10236 = CYLINDRICAL_SURFACE ( 'NONE', #8627, 0.5000000000000001110 ) ;
#10237 = ORIENTED_EDGE ( 'NONE', *, *, #9332, .F. ) ;
#10238 = DIRECTION ( 'NONE',  ( 1.000000000000000000, 0.000000000000000000, 0.000000000000000000 ) ) ;
#10239 = AXIS2_PLACEMENT_3D ( 'NONE', #5672, #10490, #12843 ) ;
#10240 = CARTESIAN_POINT ( 'NONE',  ( -198.4250122012724660, 129.4766065029076003, 7.918248976830634334 ) ) ;
#10241 = CARTESIAN_POINT ( 'NONE',  ( 114.0000000000000568, 64.53993994372673626, 15.00000000000035172 ) ) ;
#10242 = FACE_OUTER_BOUND ( 'NONE', #3022, .T. ) ;
#10243 = VERTEX_POINT ( 'NONE', #15370 ) ;
#10244 = DIRECTION ( 'NONE',  ( 1.000000000000000000, 0.000000000000000000, 0.000000000000000000 ) ) ;
#10245 = VERTEX_POINT ( 'NONE', #7033 ) ;
#10246 = ORIENTED_EDGE ( 'NONE', *, *, #11651, .F. ) ;
#10247 = FACE_OUTER_BOUND ( 'NONE', #12691, .T. ) ;
#10248 = PLANE ( 'NONE',  #177 ) ;
#10249 = DIRECTION ( 'NONE',  ( -0.000000000000000000, 1.000000000000000000, 1.156482317317871725E-16 ) ) ;
#10250 = CARTESIAN_POINT ( 'NONE',  ( -170.8822437509192582, 122.0703082676180884, 9.852955625550796626 ) ) ;
#10251 = CARTESIAN_POINT ( 'NONE',  ( -218.1232943690431512, 152.3955998793410913, -3.540502677712229929 ) ) ;
#10252 = CARTESIAN_POINT ( 'NONE',  ( -38.29899788034578734, 48.72489408690345414, 9.975000000000001421 ) ) ;
#10253 = AXIS2_PLACEMENT_3D ( 'NONE', #3862, #285, #6396 ) ;
#10254 = AXIS2_PLACEMENT_3D ( 'NONE', #9460, #8365, #11825 ) ;
#10255 = CARTESIAN_POINT ( 'NONE',  ( -85.27455057502459113, 65.19100426474074084, -20.00000000000000000 ) ) ;
#10256 = DIRECTION ( 'NONE',  ( 0.000000000000000000, 0.000000000000000000, 1.000000000000000000 ) ) ;
#10257 = EDGE_CURVE ( 'NONE', #13079, #12092, #7117, .T. ) ;
#10258 = SHAPE_REPRESENTATION ( 'Handle Balance Weight Counterbalance', ( #12337 ), #10297 ) ;
#10259 = CARTESIAN_POINT ( 'NONE',  ( -136.1405586187959784, 108.3975249866138739, 5.000000000000000000 ) ) ;
#10260 = CARTESIAN_POINT ( 'NONE',  ( -222.3080144202391466, 148.9395084873720521, -3.019567288535963900 ) ) ;
#10261 = ORIENTED_EDGE ( 'NONE', *, *, #4084, .T. ) ;
#10262 = CARTESIAN_POINT ( 'NONE',  ( -217.8617492717439461, 152.8708317265722201, 7.945910111307878054 ) ) ;
#10263 = ORIENTED_EDGE ( 'NONE', *, *, #9109, .F. ) ;
#10264 = CARTESIAN_POINT ( 'NONE',  ( 0.000000000000000000, -6.928203230275514990, -4.000000000000003553 ) ) ;
#10265 = DIRECTION ( 'NONE',  ( 0.000000000000000000, -1.000000000000000000, 0.000000000000000000 ) ) ;
#10266 = VERTEX_POINT ( 'NONE', #930 ) ;
#10267 = FACE_BOUND ( 'NONE', #12503, .T. ) ;
#10268 = CARTESIAN_POINT ( 'NONE',  ( 64.00000000000005684, 64.53993994372673626, 13.30000000000070948 ) ) ;
#10269 = EDGE_CURVE ( 'NONE', #11085, #7996, #11916, .T. ) ;
#10270 = CARTESIAN_POINT ( 'NONE',  ( 178.0000000000000853, 16.03993994372673981, 24.94742576086838781 ) ) ;
#10271 = EDGE_LOOP ( 'NONE', ( #14189, #8227, #3406, #958 ) ) ;
#10272 = CONTEXT_DEPENDENT_SHAPE_REPRESENTATION ( #3217, #6771 ) ;
#10273 = EDGE_LOOP ( 'NONE', ( #3103, #5382, #2874 ) ) ;
#10274 = CARTESIAN_POINT ( 'NONE',  ( 190.6753907620029054, 48.10438271498464502, -4.747728522856008659 ) ) ;
#10275 = DIRECTION ( 'NONE',  ( 0.000000000000000000, 0.1391731009600592484, 0.9902680687415712502 ) ) ;
#10276 = EDGE_LOOP ( 'NONE', ( #14517, #8750, #8315, #1922 ) ) ;
#10277 = DIRECTION ( 'NONE',  ( 0.000000000000000000, 0.000000000000000000, -1.000000000000000000 ) ) ;
#10278 = CARTESIAN_POINT ( 'NONE',  ( 0.2456200930617507272, -1.587713240271640958, -2.750000000000000888 ) ) ;
#10279 = ORIENTED_EDGE ( 'NONE', *, *, #859, .F. ) ;
#10280 = ORIENTED_EDGE ( 'NONE', *, *, #14988, .T. ) ;
#10281 = CARTESIAN_POINT ( 'NONE',  ( 174.2293059057019775, 61.25683321636181233, 7.600000000000002309 ) ) ;
#10282 = EDGE_CURVE ( 'NONE', #2947, #11184, #5684, .T. ) ;
#10283 = CARTESIAN_POINT ( 'NONE',  ( -85.99999999999994316, 59.53993994372674337, 15.00000000000174794 ) ) ;
#10284 = ORIENTED_EDGE ( 'NONE', *, *, #3586, .F. ) ;
#10285 = VECTOR ( 'NONE', #5836, 1000.000000000000000 ) ;
#10286 = CARTESIAN_POINT ( 'NONE',  ( 0.01688885742777249468, -6.535341423375579772, 4.680456609904006804 ) ) ;
#10287 = CARTESIAN_POINT ( 'NONE',  ( -156.6477983077465410, 110.1970436846185066, 5.000000000000004441 ) ) ;
#10288 = AXIS2_PLACEMENT_3D ( 'NONE', #5676, #10804, #15593 ) ;
#10289 = CARTESIAN_POINT ( 'NONE',  ( 64.00000000000005684, 64.53993994372673626, 15.00000000000070166 ) ) ;
#10290 = FACE_BOUND ( 'NONE', #5453, .T. ) ;
#10291 = EDGE_CURVE ( 'NONE', #6229, #1785, #13645, .T. ) ;
#10292 = EDGE_CURVE ( 'NONE', #12061, #4465, #4485, .T. ) ;
#10293 = LINE ( 'NONE', #4592, #14856 ) ;
#10294 = EDGE_CURVE ( 'NONE', #4152, #2386, #5994, .T. ) ;
#10295 = CIRCLE ( 'NONE', #6518, 1.700000000000007061 ) ;
#10296 = CARTESIAN_POINT ( 'NONE',  ( 162.8297652159045015, 17.20175482153034707, -6.370175303308202253 ) ) ;
#10297 =( GEOMETRIC_REPRESENTATION_CONTEXT ( 3 ) GLOBAL_UNCERTAINTY_ASSIGNED_CONTEXT ( ( #5949 ) ) GLOBAL_UNIT_ASSIGNED_CONTEXT ( ( #13157, #14497, #2434 ) ) REPRESENTATION_CONTEXT ( 'NONE', 'WORKASPACE' ) );
#10298 = VERTEX_POINT ( 'NONE', #9318 ) ;
#10299 = CARTESIAN_POINT ( 'NONE',  ( 114.0000000000000568, 64.53993994372673626, 15.00000000000035172 ) ) ;
#10300 = AXIS2_PLACEMENT_3D ( 'NONE', #1461, #1317, #6300 ) ;
#10301 = CARTESIAN_POINT ( 'NONE',  ( -201.8614823352862970, 146.6162971164513635, 1.515441477536285220 ) ) ;
#10302 = CARTESIAN_POINT ( 'NONE',  ( 70.26535645333922275, 38.79159067395544014, 7.600000000000002309 ) ) ;
#10303 = VERTEX_POINT ( 'NONE', #12933 ) ;
#10304 = CARTESIAN_POINT ( 'NONE',  ( -214.8265656857867327, 135.2606554265309740, 3.478895870929493483 ) ) ;
#10305 = CARTESIAN_POINT ( 'NONE',  ( 209.6520103264654438, 47.93571987055528183, -2.624305162434556582 ) ) ;
#10306 = ORIENTED_EDGE ( 'NONE', *, *, #6120, .F. ) ;
#10307 = EDGE_CURVE ( 'NONE', #899, #8731, #10128, .T. ) ;
#10308 = VECTOR ( 'NONE', #11083, 1000.000000000000114 ) ;
#10309 = DIRECTION ( 'NONE',  ( 0.000000000000000000, 0.000000000000000000, -1.000000000000000000 ) ) ;
#10310 = DIRECTION ( 'NONE',  ( -1.000000000000000000, 0.000000000000000000, 0.000000000000000000 ) ) ;
#10311 = EDGE_CURVE ( 'NONE', #15212, #4169, #2202, .T. ) ;
#10312 = CARTESIAN_POINT ( 'NONE',  ( -224.2094369203935003, 145.5328116053612746, 8.507951946043531777 ) ) ;
#10313 = CARTESIAN_POINT ( 'NONE',  ( 114.0000000000000568, 56.53993994372675047, 15.00000000000035172 ) ) ;
#10314 = CARTESIAN_POINT ( 'NONE',  ( -168.8345777152483151, 119.5835126658289909, 2.431557144026069928 ) ) ;
#10315 = EDGE_LOOP ( 'NONE', ( #8826, #4822 ) ) ;
#10316 = DIRECTION ( 'NONE',  ( -0.000000000000000000, -0.000000000000000000, 1.000000000000000000 ) ) ;
#10317 = CARTESIAN_POINT ( 'NONE',  ( -214.7423002846986151, 145.5292334337732711, 10.16010209732751335 ) ) ;
#10318 = DIRECTION ( 'NONE',  ( -0.000000000000000000, 1.000000000000000000, -0.000000000000000000 ) ) ;
#10319 = AXIS2_PLACEMENT_3D ( 'NONE', #2850, #2614, #6330 ) ;
#10320 = CARTESIAN_POINT ( 'NONE',  ( -64.00000000000002842, -178.8058001507315566, -30.31842631998718574 ) ) ;
#10321 = EDGE_LOOP ( 'NONE', ( #5587, #12171, #12712, #12251 ) ) ;
#10322 = DIRECTION ( 'NONE',  ( 1.000000000000000000, 0.000000000000000000, 0.000000000000000000 ) ) ;
#10323 = AXIS2_PLACEMENT_3D ( 'NONE', #14842, #4037, #13741 ) ;
#10324 = EDGE_CURVE ( 'NONE', #14668, #4290, #3317, .T. ) ;
#10325 = EDGE_LOOP ( 'NONE', ( #12262, #7743, #1935, #9350 ) ) ;
#10326 = ORIENTED_EDGE ( 'NONE', *, *, #4176, .T. ) ;
#10327 = CARTESIAN_POINT ( 'NONE',  ( 6.399999999999999467, 0.000000000000000000, 8.000000000000000000 ) ) ;
#10328 = CARTESIAN_POINT ( 'NONE',  ( 184.0000000000000568, -181.3058001507315566, 76.45141194869098911 ) ) ;
#10329 = CARTESIAN_POINT ( 'NONE',  ( 185.1062858801516882, 25.86394065090268057, 18.00000000000000355 ) ) ;
#10330 = CARTESIAN_POINT ( 'NONE',  ( -169.0248613439241012, 125.3981004096062435, 8.301827530276908007 ) ) ;
#10331 = CARTESIAN_POINT ( 'NONE',  ( -219.6200563870737597, 153.7554072420239493, 0.2735799754665275696 ) ) ;
#10332 = DIRECTION ( 'NONE',  ( 0.000000000000000000, 1.000000000000000000, 0.000000000000000000 ) ) ;
#10333 = DIRECTION ( 'NONE',  ( 1.000000000000000000, 0.000000000000000000, 0.000000000000000000 ) ) ;
#10334 = DIRECTION ( 'NONE',  ( 0.000000000000000000, -1.000000000000000000, -1.156482317317871478E-16 ) ) ;
#10335 = CYLINDRICAL_SURFACE ( 'NONE', #10457, 1.000000000000000888 ) ;
#10336 = FACE_OUTER_BOUND ( 'NONE', #14285, .T. ) ;
#10337 = EDGE_CURVE ( 'NONE', #12471, #14091, #2675, .T. ) ;
#10338 = AXIS2_PLACEMENT_3D ( 'NONE', #14325, #9457, #14254 ) ;
#10339 = DIRECTION ( 'NONE',  ( -0.000000000000000000, 6.938893903907227145E-17, -1.000000000000000000 ) ) ;
#10340 = VERTEX_POINT ( 'NONE', #7268 ) ;
#10341 = AXIS2_PLACEMENT_3D ( 'NONE', #14937, #2883, #11639 ) ;
#10342 = ORIENTED_EDGE ( 'NONE', *, *, #9312, .F. ) ;
#10343 = CARTESIAN_POINT ( 'NONE',  ( 70.26535645333922275, 38.79159067395544014, 9.975000000000001421 ) ) ;
#10344 = CIRCLE ( 'NONE', #3535, 0.5000000000000004441 ) ;
#10345 = CARTESIAN_POINT ( 'NONE',  ( 185.1062858801516882, 25.86394065090268057, 18.00000000000000355 ) ) ;
#10346 = FACE_OUTER_BOUND ( 'NONE', #1846, .T. ) ;
#10347 = DIRECTION ( 'NONE',  ( 0.000000000000000000, 0.000000000000000000, 1.000000000000000000 ) ) ;
#10348 = CIRCLE ( 'NONE', #2525, 1.000000000000000888 ) ;
#10349 = CARTESIAN_POINT ( 'NONE',  ( -76.00000000000001421, -179.3058001507315566, -17.19066787724516843 ) ) ;
#10350 = ORIENTED_EDGE ( 'NONE', *, *, #10257, .F. ) ;
#10351 = VECTOR ( 'NONE', #2496, 999.9999999999998863 ) ;
#10352 = AXIS2_PLACEMENT_3D ( 'NONE', #11333, #10078, #494 ) ;
#10353 = ORIENTED_EDGE ( 'NONE', *, *, #4754, .T. ) ;
#10354 = CARTESIAN_POINT ( 'NONE',  ( 211.8867585259220050, 39.31811064754020890, -6.135149402309513000 ) ) ;
#10355 = VERTEX_POINT ( 'NONE', #52 ) ;
#10356 = CARTESIAN_POINT ( 'NONE',  ( 178.0000000000000853, -178.8058001507315566, -17.19066787724516843 ) ) ;
#10357 = CARTESIAN_POINT ( 'NONE',  ( -223.6213244275821808, 142.0005027430226221, 2.566813877387965626 ) ) ;
#10358 = AXIS2_PLACEMENT_3D ( 'NONE', #5455, #12936, #15141 ) ;
#10359 = ORIENTED_EDGE ( 'NONE', *, *, #7587, .T. ) ;
#10360 = ORIENTED_EDGE ( 'NONE', *, *, #14574, .T. ) ;
#10361 = DIRECTION ( 'NONE',  ( 0.000000000000000000, -0.1391731009600660485, -0.9902680687415702510 ) ) ;
#10362 = PLANE ( 'NONE',  #13126 ) ;
#10363 = AXIS2_PLACEMENT_3D ( 'NONE', #5736, #10479, #10244 ) ;
#10364 = ORIENTED_EDGE ( 'NONE', *, *, #7671, .T. ) ;
#10365 = CARTESIAN_POINT ( 'NONE',  ( 194.7891036845171300, 47.85977741052224133, -6.433373108600371815 ) ) ;
#10366 = DIRECTION ( 'NONE',  ( 0.000000000000000000, 0.000000000000000000, -1.000000000000000000 ) ) ;
#10367 = DIRECTION ( 'NONE',  ( 1.000000000000000000, 0.000000000000000000, 0.000000000000000000 ) ) ;
#10368 = CARTESIAN_POINT ( 'NONE',  ( 17.41029453487719181, 40.04259805664093363, 10.00000000000000178 ) ) ;
#10369 = DIRECTION ( 'NONE',  ( -0.000000000000000000, -0.000000000000000000, 1.000000000000000000 ) ) ;
#10370 = EDGE_CURVE ( 'NONE', #5430, #8637, #11386, .T. ) ;
#10371 = CIRCLE ( 'NONE', #1034, 0.5000000000000069944 ) ;
#10372 = DIRECTION ( 'NONE',  ( 1.000000000000000000, 0.000000000000000000, -0.000000000000000000 ) ) ;
#10373 = AXIS2_PLACEMENT_3D ( 'NONE', #11176, #327, #5167 ) ;
#10374 = ORIENTED_EDGE ( 'NONE', *, *, #7358, .T. ) ;
#10375 = DIRECTION ( 'NONE',  ( 0.000000000000000000, 0.000000000000000000, 1.000000000000000000 ) ) ;
#10376 = EDGE_CURVE ( 'NONE', #2480, #10747, #6156, .T. ) ;
#10377 = CARTESIAN_POINT ( 'NONE',  ( -215.0356418556126812, 153.5741063705486908, -0.4547266291960771478 ) ) ;
#10378 = CARTESIAN_POINT ( 'NONE',  ( 207.1062858801516597, 40.86394065090267702, 18.00000000000001066 ) ) ;
#10379 = VERTEX_POINT ( 'NONE', #12066 ) ;
#10380 = CARTESIAN_POINT ( 'NONE',  ( -220.7908126485560274, 143.2766720833714089, -2.964974570226855288 ) ) ;
#10381 = CARTESIAN_POINT ( 'NONE',  ( 211.9051874564029561, 39.35763625820981559, -9.133132850359100274 ) ) ;
#10382 = VERTEX_POINT ( 'NONE', #9781 ) ;
#10383 = AXIS2_PLACEMENT_3D ( 'NONE', #15391, #5775, #7286 ) ;
#10384 = DIRECTION ( 'NONE',  ( 1.000000000000000000, 0.000000000000000000, 0.000000000000000000 ) ) ;
#10385 = CARTESIAN_POINT ( 'NONE',  ( 2.000000000000000000, 1.587713240271470427, 2.750000000000000888 ) ) ;
#10386 = AXIS2_PLACEMENT_3D ( 'NONE', #9625, #5989, #1160 ) ;
#10387 = FACE_BOUND ( 'NONE', #14172, .T. ) ;
#10388 = DIRECTION ( 'NONE',  ( 0.9956600981502441439, -0.09306432695424346480, -2.696501421120446373E-17 ) ) ;
#10389 = ORIENTED_EDGE ( 'NONE', *, *, #7218, .F. ) ;
#10390 = AXIS2_PLACEMENT_3D ( 'NONE', #8693, #13483, #1568 ) ;
#10391 = CYLINDRICAL_SURFACE ( 'NONE', #2899, 0.5000000000000001110 ) ;
#10392 = EDGE_CURVE ( 'NONE', #10665, #11835, #10632, .T. ) ;
#10393 = EDGE_CURVE ( 'NONE', #13605, #8345, #11042, .T. ) ;
#10394 = EDGE_CURVE ( 'NONE', #12187, #4995, #6878, .T. ) ;
#10395 = CARTESIAN_POINT ( 'NONE',  ( -195.8085210632896178, 134.3768662836672547, 10.16010209732750269 ) ) ;
#10396 = DIRECTION ( 'NONE',  ( 0.000000000000000000, 1.000000000000000000, 0.000000000000000000 ) ) ;
#10397 = VECTOR ( 'NONE', #8597, 1000.000000000000000 ) ;
#10398 = LINE ( 'NONE', #11578, #12838 ) ;
#10399 = VERTEX_POINT ( 'NONE', #13316 ) ;
#10400 = CARTESIAN_POINT ( 'NONE',  ( 10.39230484541326582, 0.000000000000000000, 0.000000000000000000 ) ) ;
#10401 = ORIENTED_EDGE ( 'NONE', *, *, #2770, .T. ) ;
#10402 = ORIENTED_EDGE ( 'NONE', *, *, #1077, .T. ) ;
#10403 = DIRECTION ( 'NONE',  ( 0.000000000000000000, 0.000000000000000000, 1.000000000000000000 ) ) ;
#10404 = LINE ( 'NONE', #9224, #14800 ) ;
#10405 = CARTESIAN_POINT ( 'NONE',  ( 185.1062858801516882, 25.86394065090268057, 13.00000000000000178 ) ) ;
#10406 = CARTESIAN_POINT ( 'NONE',  ( -172.6089438593484147, 118.9766539771727452, 8.890414347921929306 ) ) ;
#10407 = CARTESIAN_POINT ( 'NONE',  ( -223.5023877967964268, 146.7996010982761845, -2.058674291180297100 ) ) ;
#10408 = DIRECTION ( 'NONE',  ( 0.000000000000000000, 0.000000000000000000, -1.000000000000000000 ) ) ;
#10410 = PRESENTATION_LAYER_ASSIGNMENT (  '', '', ( #15177 ) ) ;
#10409 = CONICAL_SURFACE ( 'NONE', #11919, 3.525000000000000355, 0.7853981633975176679 ) ;
#10411 = ADVANCED_FACE ( 'NONE', ( #4889 ), #3860, .T. ) ;
#10412 = DIRECTION ( 'NONE',  ( 0.000000000000000000, -1.000000000000000000, -1.156482317317871478E-16 ) ) ;
#10413 = FACE_OUTER_BOUND ( 'NONE', #15116, .T. ) ;
#10414 = DIRECTION ( 'NONE',  ( 0.000000000000000000, 0.000000000000000000, -1.000000000000000000 ) ) ;
#10415 = CARTESIAN_POINT ( 'NONE',  ( 114.0000000000000568, 64.53993994372673626, 15.00000000000035172 ) ) ;
#10416 = CARTESIAN_POINT ( 'NONE',  ( -224.1052059537137495, 145.7195577436698954, -0.7975646616046745407 ) ) ;
#10417 = ORIENTED_EDGE ( 'NONE', *, *, #12338, .T. ) ;
#10418 = EDGE_LOOP ( 'NONE', ( #2709, #6604, #9256, #15016 ) ) ;
#10419 = DIRECTION ( 'NONE',  ( 0.000000000000000000, -1.000000000000000000, -4.956352788505162775E-17 ) ) ;
#10420 = CARTESIAN_POINT ( 'NONE',  ( 177.5000000000000853, 19.53993994372673626, 52.49999999999997868 ) ) ;
#10421 = AXIS2_PLACEMENT_3D ( 'NONE', #6945, #9161, #6641 ) ;
#10422 = ORIENTED_EDGE ( 'NONE', *, *, #4891, .F. ) ;
#10423 = CARTESIAN_POINT ( 'NONE',  ( 5.799999999999999822, 6.928203230275487456, 4.000000000000003553 ) ) ;
#10424 = CARTESIAN_POINT ( 'NONE',  ( 0.000000000000000000, -7.511572993685817836E-16, 2.749999999999999112 ) ) ;
#10425 = PRODUCT ( 'hex bolt gradeb_iso_ISO 4015 - M3 x 20 x 12-N', 'hex bolt gradeb_iso_ISO 4015 - M3 x 20 x 12-N', '', ( #8348 ) ) ;
#10426 = AXIS2_PLACEMENT_3D ( 'NONE', #8283, #13062, #15200 ) ;
#10427 = EDGE_CURVE ( 'NONE', #10711, #3709, #13399, .T. ) ;
#10428 = EDGE_CURVE ( 'NONE', #3793, #13203, #9869, .T. ) ;
#10429 = DIRECTION ( 'NONE',  ( 0.000000000000000000, 1.000000000000000000, 6.938893903907227145E-17 ) ) ;
#10430 = VERTEX_POINT ( 'NONE', #1393 ) ;
#10431 = ADVANCED_FACE ( 'NONE', ( #3932 ), #42, .T. ) ;
#10432 = SHAPE_DEFINITION_REPRESENTATION ( #1706, #556 ) ;
#10433 = ORIENTED_EDGE ( 'NONE', *, *, #6575, .F. ) ;
#10434 = VECTOR ( 'NONE', #1483, 1000.000000000000000 ) ;
#10435 = CARTESIAN_POINT ( 'NONE',  ( 204.0369835420791276, 51.66931235154874003, -2.492621690445610216 ) ) ;
#10436 = FILL_AREA_STYLE_COLOUR ( '', #11640 ) ;
#10437 = VERTEX_POINT ( 'NONE', #6310 ) ;
#10438 = DIRECTION ( 'NONE',  ( 1.000000000000000000, 0.000000000000000000, 0.000000000000000000 ) ) ;
#10439 = AXIS2_PLACEMENT_3D ( 'NONE', #11494, #5798, #10534 ) ;
#10440 = CYLINDRICAL_SURFACE ( 'NONE', #14598, 4.499999999999950262 ) ;
#10441 = ORIENTED_EDGE ( 'NONE', *, *, #7642, .T. ) ;
#10442 = ORIENTED_EDGE ( 'NONE', *, *, #6061, .T. ) ;
#10443 = DIRECTION ( 'NONE',  ( -1.000000000000000000, 0.000000000000000000, 0.000000000000000000 ) ) ;
#10444 = DIRECTION ( 'NONE',  ( -0.000000000000000000, 0.000000000000000000, 1.000000000000000000 ) ) ;
#10445 = ORIENTED_EDGE ( 'NONE', *, *, #8690, .T. ) ;
#10446 = DIRECTION ( 'NONE',  ( -0.000000000000000000, -0.000000000000000000, 1.000000000000000000 ) ) ;
#10447 = CIRCLE ( 'NONE', #8188, 1.499999999999997780 ) ;
#10448 = PLANE ( 'NONE',  #13602 ) ;
#10449 = DIRECTION ( 'NONE',  ( -1.000000000000000000, -0.000000000000000000, -0.000000000000000000 ) ) ;
#10450 = EDGE_CURVE ( 'NONE', #13870, #7084, #194, .T. ) ;
#10451 = LINE ( 'NONE', #4435, #8407 ) ;
#10452 = CIRCLE ( 'NONE', #10962, 0.5000000000000004441 ) ;
#10453 = DIRECTION ( 'NONE',  ( 0.000000000000000000, 0.000000000000000000, 1.000000000000000000 ) ) ;
#10454 = ORIENTED_EDGE ( 'NONE', *, *, #3981, .T. ) ;
#10455 = ADVANCED_FACE ( 'NONE', ( #3621 ), #2437, .F. ) ;
#10456 = PLANE ( 'NONE',  #15492 ) ;
#10457 = AXIS2_PLACEMENT_3D ( 'NONE', #11679, #9233, #8143 ) ;
#10458 = CARTESIAN_POINT ( 'NONE',  ( -198.5633888957220563, 144.7754908190922549, 1.515441477536285442 ) ) ;
#10459 = CARTESIAN_POINT ( 'NONE',  ( 167.9295236634097819, 65.51901744756737855, -0.9107274384406879308 ) ) ;
#10460 = VERTEX_POINT ( 'NONE', #282 ) ;
#10461 = CARTESIAN_POINT ( 'NONE',  ( -205.7712766299887335, 131.5939592662764994, -0.4555467707853333992 ) ) ;
#10462 = CARTESIAN_POINT ( 'NONE',  ( 193.0268458394156710, 50.40397125358524733, -1.873914241081319210 ) ) ;
#10463 = VERTEX_POINT ( 'NONE', #1241 ) ;
#10464 = EDGE_CURVE ( 'NONE', #5369, #3026, #3326, .T. ) ;
#10465 = CARTESIAN_POINT ( 'NONE',  ( -35.99999999999995026, 62.13993994372673768, 16.70000000000140261 ) ) ;
#10466 = CARTESIAN_POINT ( 'NONE',  ( -5.196152422706636465, 9.000000000000001776, 5.000000000000000000 ) ) ;
#10467 = DIRECTION ( 'NONE',  ( 0.000000000000000000, 0.000000000000000000, 1.000000000000000000 ) ) ;
#10468 = AXIS2_PLACEMENT_3D ( 'NONE', #4382, #7801, #10238 ) ;
#10469 = ADVANCED_FACE ( 'NONE', ( #9945 ), #6925, .F. ) ;
#10470 = ORIENTED_EDGE ( 'NONE', *, *, #10282, .F. ) ;
#10471 = DIRECTION ( 'NONE',  ( 0.000000000000000000, 0.000000000000000000, 1.000000000000000000 ) ) ;
#10472 = CARTESIAN_POINT ( 'NONE',  ( 190.0000000000000568, -179.8058001507315566, -30.31842631998718574 ) ) ;
#10473 = ORIENTED_EDGE ( 'NONE', *, *, #8276, .F. ) ;
#10474 = DIRECTION ( 'NONE',  ( 0.000000000000000000, -1.000000000000000000, -6.938893903907227145E-17 ) ) ;
#10475 = CARTESIAN_POINT ( 'NONE',  ( -197.2254974982137128, 131.7248478061943615, 9.577123744044225617 ) ) ;
#10476 = LINE ( 'NONE', #10630, #8535 ) ;
#10477 = DIRECTION ( 'NONE',  ( -1.000000000000000000, 0.000000000000000000, 0.000000000000000000 ) ) ;
#10478 = ORIENTED_EDGE ( 'NONE', *, *, #1989, .F. ) ;
#10479 = DIRECTION ( 'NONE',  ( 0.000000000000000000, 0.000000000000000000, 1.000000000000000000 ) ) ;
#10480 = ORIENTED_EDGE ( 'NONE', *, *, #4971, .T. ) ;
#10481 = ORIENTED_EDGE ( 'NONE', *, *, #10773, .T. ) ;
#10482 = DIRECTION ( 'NONE',  ( 0.000000000000000000, -1.000000000000000000, -6.938893903907222067E-15 ) ) ;
#10483 = DIRECTION ( 'NONE',  ( 3.965082230804130220E-16, -1.486905836551548832E-16, 1.000000000000000000 ) ) ;
#10484 = CARTESIAN_POINT ( 'NONE',  ( 154.0873337668446368, 6.722585725381706290, -7.588739505787663653 ) ) ;
#10485 = CARTESIAN_POINT ( 'NONE',  ( -170.6576934677675581, 122.4726253483332812, 9.815104126961024633 ) ) ;
#10486 = CARTESIAN_POINT ( 'NONE',  ( -222.7865639444310943, 148.0821118951906215, -4.926004749479361955 ) ) ;
#10487 = ADVANCED_FACE ( 'NONE', ( #15418 ), #4490, .T. ) ;
#10489 = EDGE_CURVE ( 'NONE', #13181, #12329, #1047, .T. ) ;
#10488 = EDGE_CURVE ( 'NONE', #2142, #2861, #4094, .T. ) ;
#10490 = DIRECTION ( 'NONE',  ( -0.8863182623094566503, 0.4630766004634062072, 0.000000000000000000 ) ) ;
#10491 = CARTESIAN_POINT ( 'NONE',  ( -110.0000000000000426, 19.53993994372674337, 9.999999999999998224 ) ) ;
#10492 = EDGE_CURVE ( 'NONE', #11360, #6077, #5098, .T. ) ;
#10493 = DIRECTION ( 'NONE',  ( 1.000000000000000000, 0.000000000000000000, 0.000000000000000000 ) ) ;
#10494 = VECTOR ( 'NONE', #5006, 1000.000000000000000 ) ;
#10495 = DIRECTION ( 'NONE',  ( -0.000000000000000000, -0.000000000000000000, -1.000000000000000000 ) ) ;
#10496 = CARTESIAN_POINT ( 'NONE',  ( 178.0000000000000853, 11.87216911405866959, 26.40245448993442068 ) ) ;
#10497 = EDGE_LOOP ( 'NONE', ( #6192, #13707, #15419, #12267 ) ) ;
#10498 = ORIENTED_EDGE ( 'NONE', *, *, #5403, .T. ) ;
#10499 = LINE ( 'NONE', #15137, #9308 ) ;
#10500 = VERTEX_POINT ( 'NONE', #2762 ) ;
#10501 = FACE_OUTER_BOUND ( 'NONE', #1830, .T. ) ;
#10502 = CARTESIAN_POINT ( 'NONE',  ( 177.5000000000000853, 16.03993994372673981, -3.075184203610571654 ) ) ;
#10503 = AXIS2_PLACEMENT_3D ( 'NONE', #2423, #7179, #5979 ) ;
#10504 = EDGE_CURVE ( 'NONE', #11537, #10667, #9003, .T. ) ;
#10505 = DIRECTION ( 'NONE',  ( -1.000000000000000000, -1.669238443041287429E-16, 0.000000000000000000 ) ) ;
#10506 = ORIENTED_EDGE ( 'NONE', *, *, #5254, .T. ) ;
#10507 = ORIENTED_EDGE ( 'NONE', *, *, #2003, .T. ) ;
#10508 = EDGE_CURVE ( 'NONE', #10243, #9525, #14974, .T. ) ;
#10509 = DIRECTION ( 'NONE',  ( -0.000000000000000000, -0.000000000000000000, 1.000000000000000000 ) ) ;
#10510 = ORIENTED_EDGE ( 'NONE', *, *, #9175, .F. ) ;
#10511 = FACE_OUTER_BOUND ( 'NONE', #7472, .T. ) ;
#10512 = FACE_OUTER_BOUND ( 'NONE', #8280, .T. ) ;
#10513 = ORIENTED_EDGE ( 'NONE', *, *, #8761, .T. ) ;
#10514 = ORIENTED_EDGE ( 'NONE', *, *, #3537, .F. ) ;
#10515 = LINE ( 'NONE', #11707, #14566 ) ;
#10516 = CYLINDRICAL_SURFACE ( 'NONE', #13138, 0.5000000000000004441 ) ;
#10517 = EDGE_CURVE ( 'NONE', #14746, #2220, #5609, .T. ) ;
#10518 = EDGE_LOOP ( 'NONE', ( #13098, #12244, #10051, #6187 ) ) ;
#10519 = DIRECTION ( 'NONE',  ( 0.4999999999999997224, 0.8660254037844387076, 0.000000000000000000 ) ) ;
#10520 = AXIS2_PLACEMENT_3D ( 'NONE', #14965, #13632, #11354 ) ;
#10521 = DIRECTION ( 'NONE',  ( -0.000000000000000000, -0.000000000000000000, 1.000000000000000000 ) ) ;
#10522 = CARTESIAN_POINT ( 'NONE',  ( 0.7145311798163258565, 9.237604307034018802, 0.000000000000000000 ) ) ;
#10523 = ORIENTED_EDGE ( 'NONE', *, *, #1251, .F. ) ;
#10524 = DIRECTION ( 'NONE',  ( -0.000000000000000000, 0.9902680687415712502, 0.1391731009600584990 ) ) ;
#10525 = CARTESIAN_POINT ( 'NONE',  ( 190.0000000000000568, -178.8058001507315566, -17.19066787724516843 ) ) ;
#10526 = CARTESIAN_POINT ( 'NONE',  ( -70.00000000000000000, 15.53993994372673981, -12.49999999999999289 ) ) ;
#10527 = ORIENTED_EDGE ( 'NONE', *, *, #2163, .F. ) ;
#10528 = CARTESIAN_POINT ( 'NONE',  ( -207.1238489746795608, 137.1336079999123854, -4.642206099735007641 ) ) ;
#10529 = UNCERTAINTY_MEASURE_WITH_UNIT (LENGTH_MEASURE( 1.000000000000000082E-05 ), #15547, 'distance_accuracy_value', 'NONE');
#10530 = CARTESIAN_POINT ( 'NONE',  ( 198.3593989614203963, 52.60648038231462920, -8.258707374242266752 ) ) ;
#10531 = AXIS2_PLACEMENT_3D ( 'NONE', #3219, #12845, #10493 ) ;
#10532 = ORIENTED_EDGE ( 'NONE', *, *, #7803, .T. ) ;
#10533 = EDGE_CURVE ( 'NONE', #4972, #2866, #3838, .T. ) ;
#10534 = DIRECTION ( 'NONE',  ( 0.000000000000000000, 0.000000000000000000, -1.000000000000000000 ) ) ;
#10535 = DIRECTION ( 'NONE',  ( 1.000000000000000000, -0.000000000000000000, -0.000000000000000000 ) ) ;
#10536 = CARTESIAN_POINT ( 'NONE',  ( 190.0000000000000853, 15.03993994372673804, 38.07518420361041933 ) ) ;
#10537 = AXIS2_PLACEMENT_3D ( 'NONE', #10328, #4155, #1791 ) ;
#10538 = EDGE_LOOP ( 'NONE', ( #7523, #8189, #11424, #12397 ) ) ;
#10539 = B_SPLINE_CURVE_WITH_KNOTS ( 'NONE', 3,
 ( #12022, #6264, #7381, #5075, #14691, #153, #7530, #6110, #14533, #8488, #12327, #1191, #1352, #9580, #13270, #3652, #3730, #11003 ),
 .UNSPECIFIED., .F., .F.,
 ( 4, 2, 2, 2, 2, 2, 2, 2, 4 ),
 ( 1.453963218420191702E-17, 0.0003981710496980498271, 0.0007963420993960851259, 0.001194513149094120425, 0.001592684198792155724, 0.001990855248490191239, 0.002389026298188226538, 0.002787197347886261837, 0.003185368397584297136 ),
 .UNSPECIFIED. ) ;
#10540 = CONICAL_SURFACE ( 'NONE', #8298, 3.525000000000000355, 0.7853981633973787790 ) ;
#10541 = CARTESIAN_POINT ( 'NONE',  ( -64.00000000000002842, -179.3058001507315566, -29.88378295107905913 ) ) ;
#10542 = CARTESIAN_POINT ( 'NONE',  ( 194.8483215340629613, 47.90965193911861775, -4.864368187704507740 ) ) ;
#10543 = ORIENTED_EDGE ( 'NONE', *, *, #12780, .F. ) ;
#10544 = DIRECTION ( 'NONE',  ( -0.000000000000000000, -0.000000000000000000, 1.000000000000000000 ) ) ;
#10545 = CARTESIAN_POINT ( 'NONE',  ( -194.3889542450793613, 137.0335258394182745, 9.578254705571838556 ) ) ;
#10546 = LINE ( 'NONE', #8275, #707 ) ;
#10547 = LINE ( 'NONE', #13297, #5554 ) ;
#10548 = PRODUCT ( 'nut M10', 'nut M10', '', ( #14394 ) ) ;
#10549 = FACE_OUTER_BOUND ( 'NONE', #10712, .T. ) ;
#10550 = EDGE_CURVE ( 'NONE', #6887, #9678, #2071, .T. ) ;
#10551 = EDGE_LOOP ( 'NONE', ( #7852, #6593, #11310, #1174 ) ) ;
#10552 = VERTEX_POINT ( 'NONE', #14816 ) ;
#10553 = LINE ( 'NONE', #4312, #9693 ) ;
#10554 = FACE_OUTER_BOUND ( 'NONE', #12703, .T. ) ;
#10555 = AXIS2_PLACEMENT_3D ( 'NONE', #3510, #2624, #14760 ) ;
#10556 = VECTOR ( 'NONE', #9604, 1000.000000000000000 ) ;
#10557 = DIRECTION ( 'NONE',  ( -0.000000000000000000, 1.000000000000000000, -0.000000000000000000 ) ) ;
#10558 = CARTESIAN_POINT ( 'NONE',  ( -168.2037493089125348, 126.8692515131764367, 6.097242495366466564 ) ) ;
#10559 = CARTESIAN_POINT ( 'NONE',  ( -223.3602385083506761, 147.0542838622007480, -2.257390889150600266 ) ) ;
#10560 = CARTESIAN_POINT ( 'NONE',  ( -216.7960616128559650, 154.7191080884769860, 4.212816267783609625 ) ) ;
#10561 = DIRECTION ( 'NONE',  ( 0.000000000000000000, 0.000000000000000000, -1.000000000000000000 ) ) ;
#10562 = AXIS2_PLACEMENT_3D ( 'NONE', #15600, #5993, #14422 ) ;
#10563 = CARTESIAN_POINT ( 'NONE',  ( -5.196152422706636465, 9.000000000000001776, 5.000000000000000000 ) ) ;
#10564 = ADVANCED_FACE ( 'NONE', ( #6485 ), #533, .T. ) ;
#10565 = AXIS2_PLACEMENT_3D ( 'NONE', #5578, #9283, #10467 ) ;
#10566 = CARTESIAN_POINT ( 'NONE',  ( 70.26535645333922275, 38.79159067395544014, 5.000000000000000000 ) ) ;
#10567 = VECTOR ( 'NONE', #12498, 1000.000000000000114 ) ;
#10568 = CARTESIAN_POINT ( 'NONE',  ( -63.50000000000002842, -181.3058001507315566, 84.88378295107885663 ) ) ;
#10569 = CARTESIAN_POINT ( 'NONE',  ( 184.0000000000000568, -179.3058001507315566, -42.95141194869119516 ) ) ;
#10570 = DIRECTION ( 'NONE',  ( -0.000000000000000000, 1.000000000000000000, 1.156482317317871725E-16 ) ) ;
#10571 = ORIENTED_EDGE ( 'NONE', *, *, #11533, .F. ) ;
#10572 = EDGE_CURVE ( 'NONE', #15023, #927, #13919, .T. ) ;
#10573 = CARTESIAN_POINT ( 'NONE',  ( -219.4360840196857509, 154.0850226169902442, 3.058976617611885107 ) ) ;
#10574 = PRODUCT_DEFINITION ( 'UNKNOWN', '', #6024, #12612 ) ;
#10575 = ORIENTED_EDGE ( 'NONE', *, *, #14000, .T. ) ;
#10576 = CARTESIAN_POINT ( 'NONE',  ( -64.00000000000002842, -179.8058001507315566, -30.31842631998718574 ) ) ;
#10577 = CARTESIAN_POINT ( 'NONE',  ( 177.5000000000000853, -178.8058001507315566, -30.31842631998718574 ) ) ;
#10578 = VERTEX_POINT ( 'NONE', #4297 ) ;
#10579 = VECTOR ( 'NONE', #14078, 1000.000000000000000 ) ;
#10580 = DIRECTION ( 'NONE',  ( -0.000000000000000000, -0.000000000000000000, 1.000000000000000000 ) ) ;
#10581 = CARTESIAN_POINT ( 'NONE',  ( 184.0000000000000568, 15.53993994372673626, 45.99999999999998579 ) ) ;
#10582 = ADVANCED_FACE ( 'NONE', ( #14009 ), #8884, .T. ) ;
#10583 = CIRCLE ( 'NONE', #12577, 0.5000000000000004441 ) ;
#10584 = ORIENTED_EDGE ( 'NONE', *, *, #1682, .T. ) ;
#10585 = AXIS2_PLACEMENT_3D ( 'NONE', #10221, #6600, #801 ) ;
#10586 = VERTEX_POINT ( 'NONE', #497 ) ;
#10587 = AXIS2_PLACEMENT_3D ( 'NONE', #10289, #13916, #3107 ) ;
#10588 = CARTESIAN_POINT ( 'NONE',  ( 207.3822464892701305, 31.45897796630539744, -3.508361229271337312 ) ) ;
#10589 = EDGE_LOOP ( 'NONE', ( #12120, #12328, #6510, #14510 ) ) ;
#10591 = CIRCLE ( 'NONE', #13096, 1.500000000000000666 ) ;
#10590 = DIRECTION ( 'NONE',  ( 1.000000000000000000, 0.000000000000000000, 0.000000000000000000 ) ) ;
#10592 = EDGE_CURVE ( 'NONE', #1358, #7962, #5653, .T. ) ;
#10593 = EDGE_CURVE ( 'NONE', #6121, #10896, #8119, .T. ) ;
#10594 = FACE_OUTER_BOUND ( 'NONE', #11718, .T. ) ;
#10595 = ADVANCED_FACE ( 'NONE', ( #11416 ), #7956, .F. ) ;
#10596 = DIRECTION ( 'NONE',  ( 0.000000000000000000, -0.1391731009600660485, -0.9902680687415702510 ) ) ;
#10597 = EDGE_LOOP ( 'NONE', ( #4690, #1789, #9358, #682 ) ) ;
#10598 = ORIENTED_EDGE ( 'NONE', *, *, #518, .T. ) ;
#10599 = DIRECTION ( 'NONE',  ( 1.000000000000000000, -2.751328491981765035E-32, 3.965082230804130220E-16 ) ) ;
#10600 = LINE ( 'NONE', #7292, #14883 ) ;
#10601 = ORIENTED_EDGE ( 'NONE', *, *, #7394, .T. ) ;
#10602 = DIRECTION ( 'NONE',  ( 0.000000000000000000, 0.9902680687415712502, 0.1391731009600596092 ) ) ;
#10603 = AXIS2_PLACEMENT_3D ( 'NONE', #14556, #9190, #12955 ) ;
#10604 = AXIS2_PLACEMENT_3D ( 'NONE', #15429, #4627, #7968 ) ;
#10605 = CARTESIAN_POINT ( 'NONE',  ( -70.00000000000000000, -179.3058001507315566, -42.95141194869119516 ) ) ;
#10606 = EDGE_LOOP ( 'NONE', ( #8601, #6906, #14438, #2297 ) ) ;
#10607 = EDGE_CURVE ( 'NONE', #7205, #3793, #12400, .T. ) ;
#10608 = ORIENTED_EDGE ( 'NONE', *, *, #9696, .F. ) ;
#10609 = CIRCLE ( 'NONE', #3295, 3.500000000000003109 ) ;
#10610 = ORIENTED_EDGE ( 'NONE', *, *, #6218, .T. ) ;
#10611 = DIRECTION ( 'NONE',  ( -0.000000000000000000, 1.000000000000000000, 2.731481088613017720E-16 ) ) ;
#10612 = CIRCLE ( 'NONE', #15130, 3.500000000000003109 ) ;
#10613 = CARTESIAN_POINT ( 'NONE',  ( -81.77455057502459113, 65.19100426474074084, 7.600000000000002309 ) ) ;
#10614 = CARTESIAN_POINT ( 'NONE',  ( 175.9483885134608272, -178.8058001507315566, 52.19066787724494816 ) ) ;
#10615 = ORIENTED_EDGE ( 'NONE', *, *, #14144, .F. ) ;
#10616 = CARTESIAN_POINT ( 'NONE',  ( -218.2851610432379346, 147.7600012847656217, -5.230826428279595319 ) ) ;
#10617 = CARTESIAN_POINT ( 'NONE',  ( 193.1446408943811548, 35.52021409135998198, -4.254410606405073736 ) ) ;
#10618 = ORIENTED_EDGE ( 'NONE', *, *, #14701, .F. ) ;
#10619 = DIRECTION ( 'NONE',  ( -1.000000000000000000, 0.000000000000000000, 0.000000000000000000 ) ) ;
#10620 = CARTESIAN_POINT ( 'NONE',  ( -33.09899788034579871, 48.72489408690345414, 0.000000000000000000 ) ) ;
#10621 = CARTESIAN_POINT ( 'NONE',  ( 184.0000000000000568, 17.53993994372673271, 45.99999999999998579 ) ) ;
#10622 = TOROIDAL_SURFACE ( 'NONE', #13624, 1.000000000000000000, 0.5000000000000000000 ) ;
#10623 = EDGE_CURVE ( 'NONE', #973, #5616, #6619, .T. ) ;
#10624 = EDGE_LOOP ( 'NONE', ( #10824, #9489, #15196, #12 ) ) ;
#10625 = DIRECTION ( 'NONE',  ( 0.9956600981502373715, -0.09306432695431542113, 0.000000000000000000 ) ) ;
#10626 = CARTESIAN_POINT ( 'NONE',  ( -85.99999999999994316, 64.53993994372673626, 15.00000000000174794 ) ) ;
#10627 = ORIENTED_EDGE ( 'NONE', *, *, #12307, .T. ) ;
#10628 = DIRECTION ( 'NONE',  ( -1.000000000000000000, 0.000000000000000000, -0.000000000000000000 ) ) ;
#10629 = CARTESIAN_POINT ( 'NONE',  ( -221.7331157600676192, 141.5908957077777188, 1.515400478619091551 ) ) ;
#10630 = CARTESIAN_POINT ( 'NONE',  ( 190.0000000000000853, 15.53993994372673804, 52.49999999999997868 ) ) ;
#10631 = CARTESIAN_POINT ( 'NONE',  ( 114.0000000000000568, 64.53993994372673626, 15.00000000000035172 ) ) ;
#10633 = CARTESIAN_POINT ( 'NONE',  ( -85.99999999999994316, 59.53993994372674337, 13.30000000000175575 ) ) ;
#10632 = CIRCLE ( 'NONE', #12637, 5.000000000000004441 ) ;
#10634 = ORIENTED_EDGE ( 'NONE', *, *, #2581, .T. ) ;
#10635 = VERTEX_POINT ( 'NONE', #4454 ) ;
#10636 = DIRECTION ( 'NONE',  ( 0.000000000000000000, 0.000000000000000000, 1.000000000000000000 ) ) ;
#10637 = CARTESIAN_POINT ( 'NONE',  ( 190.5000000000000568, 16.03993994372673981, 9.617930870223348805 ) ) ;
#10638 = FACE_OUTER_BOUND ( 'NONE', #13562, .T. ) ;
#10639 = DIRECTION ( 'NONE',  ( -1.000000000000000000, -0.000000000000000000, -0.000000000000000000 ) ) ;
#10640 = ADVANCED_FACE ( 'NONE', ( #4218, #8982 ), #9056, .T. ) ;
#10641 = CARTESIAN_POINT ( 'NONE',  ( -222.9903997373972402, 143.2271625030612086, -1.944083899231426882 ) ) ;
#10642 = EDGE_CURVE ( 'NONE', #6421, #1565, #2323, .T. ) ;
#10643 = CARTESIAN_POINT ( 'NONE',  ( -221.5485735812534358, 146.0927223962365531, 9.417135290729820696 ) ) ;
#10644 = AXIS2_PLACEMENT_3D ( 'NONE', #8603, #123, #12289 ) ;
#10645 = CARTESIAN_POINT ( 'NONE',  ( 6.800000000000000711, 6.613092715395731132E-16, 5.400000000000019007 ) ) ;
#10646 = AXIS2_PLACEMENT_3D ( 'NONE', #8145, #12848, #4718 ) ;
#10647 = DIRECTION ( 'NONE',  ( 0.000000000000000000, 0.000000000000000000, -1.000000000000000000 ) ) ;
#10648 = LINE ( 'NONE', #15438, #12963 ) ;
#10649 = CARTESIAN_POINT ( 'NONE',  ( -169.9318100387881714, 128.7846982781319412, 2.500000000781056997 ) ) ;
#10650 = CARTESIAN_POINT ( 'NONE',  ( 178.0000000000000853, 15.03993994372673804, 37.07518420361041933 ) ) ;
#10651 = DIRECTION ( 'NONE',  ( -0.000000000000000000, -0.000000000000000000, 1.000000000000000000 ) ) ;
#10652 = VERTEX_POINT ( 'NONE', #738 ) ;
#10653 = ADVANCED_FACE ( 'NONE', ( #6848 ), #12896, .T. ) ;
#10654 =( NAMED_UNIT ( * ) SI_UNIT ( $, .STERADIAN. ) SOLID_ANGLE_UNIT ( ) );
#10655 = ORIENTED_EDGE ( 'NONE', *, *, #12780, .T. ) ;
#10656 = DIRECTION ( 'NONE',  ( -0.000000000000000000, -0.000000000000000000, 1.000000000000000000 ) ) ;
#10657 = CARTESIAN_POINT ( 'NONE',  ( 122.5806775638430253, 45.00321902537314145, 5.000000000000000000 ) ) ;
#10658 =( GEOMETRIC_REPRESENTATION_CONTEXT ( 3 ) GLOBAL_UNCERTAINTY_ASSIGNED_CONTEXT ( ( #12732 ) ) GLOBAL_UNIT_ASSIGNED_CONTEXT ( ( #13281, #2330, #6924 ) ) REPRESENTATION_CONTEXT ( 'NONE', 'WORKASPACE' ) );
#10659 = DIRECTION ( 'NONE',  ( -0.000000000000000000, 1.000000000000000000, -0.000000000000000000 ) ) ;
#10660 = CARTESIAN_POINT ( 'NONE',  ( -192.1704923257120754, 141.1970532186197431, 2.500000000000000000 ) ) ;
#10661 = FACE_OUTER_BOUND ( 'NONE', #4342, .T. ) ;
#10662 = AXIS2_PLACEMENT_3D ( 'NONE', #2203, #10659, #15447 ) ;
#10663 = ORIENTED_EDGE ( 'NONE', *, *, #14711, .F. ) ;
#10664 = EDGE_CURVE ( 'NONE', #5844, #13203, #1562, .T. ) ;
#10665 = VERTEX_POINT ( 'NONE', #5420 ) ;
#10666 = CARTESIAN_POINT ( 'NONE',  ( 209.5402858782260864, 48.07700032709870896, -2.761241636875660710 ) ) ;
#10667 = VERTEX_POINT ( 'NONE', #7799 ) ;
#10668 = AXIS2_PLACEMENT_3D ( 'NONE', #4082, #5196, #280 ) ;
#10669 = FACE_OUTER_BOUND ( 'NONE', #1031, .T. ) ;
#10670 = LINE ( 'NONE', #5769, #2481 ) ;
#10671 = DIRECTION ( 'NONE',  ( -0.000000000000000000, 0.000000000000000000, 1.000000000000000000 ) ) ;
#10672 = ORIENTED_EDGE ( 'NONE', *, *, #11322, .T. ) ;
#10673 = VERTEX_POINT ( 'NONE', #10159 ) ;
#10674 = DIRECTION ( 'NONE',  ( 1.000000000000000000, -2.751328491981765035E-32, 3.965082230804130220E-16 ) ) ;
#10675 = DIRECTION ( 'NONE',  ( -0.000000000000000000, 1.486905836551548832E-16, -1.000000000000000000 ) ) ;
#10676 = AXIS2_PLACEMENT_3D ( 'NONE', #14579, #8605, #3780 ) ;
#10677 = ORIENTED_EDGE ( 'NONE', *, *, #8647, .F. ) ;
#10678 = FACE_OUTER_BOUND ( 'NONE', #13679, .T. ) ;
#10679 = FACE_OUTER_BOUND ( 'NONE', #12027, .T. ) ;
#10680 = CARTESIAN_POINT ( 'NONE',  ( 17.41029453487719181, 40.04259805664093363, 10.00000000000000178 ) ) ;
#10681 = AXIS2_PLACEMENT_3D ( 'NONE', #10255, #12611, #603 ) ;
#10682 = EDGE_CURVE ( 'NONE', #6077, #13452, #14664, .T. ) ;
#10684 = EDGE_CURVE ( 'NONE', #12934, #50, #11338, .T. ) ;
#10683 = ADVANCED_FACE ( 'NONE', ( #13858 ), #10236, .T. ) ;
#10685 = ORIENTED_EDGE ( 'NONE', *, *, #12235, .T. ) ;
#10686 = VECTOR ( 'NONE', #12375, 1000.000000000000000 ) ;
#10687 = DIRECTION ( 'NONE',  ( 1.000000000000000000, 0.000000000000000000, 0.000000000000000000 ) ) ;
#10688 = VERTEX_POINT ( 'NONE', #12585 ) ;
#10689 = DIRECTION ( 'NONE',  ( 1.000000000000000000, 0.000000000000000000, 0.000000000000000000 ) ) ;
#10690 = DIRECTION ( 'NONE',  ( -1.000000000000000000, -0.000000000000000000, -0.000000000000000000 ) ) ;
#10691 = CARTESIAN_POINT ( 'NONE',  ( 178.0000000000000853, -179.3058001507315851, 64.88378295107887084 ) ) ;
#10692 = ORIENTED_EDGE ( 'NONE', *, *, #15288, .F. ) ;
#10693 = CARTESIAN_POINT ( 'NONE',  ( -213.7219974575431252, 137.2233070386400584, -2.964974570226852180 ) ) ;
#10694 = CARTESIAN_POINT ( 'NONE',  ( 194.8602319459051557, 33.82038799488785230, -7.127215995405879134 ) ) ;
#10695 = AXIS2_PLACEMENT_3D ( 'NONE', #1457, #267, #13534 ) ;
#10696 = ORIENTED_EDGE ( 'NONE', *, *, #401, .F. ) ;
#10697 = CIRCLE ( 'NONE', #9950, 3.500000000000003109 ) ;
#10698 = DIRECTION ( 'NONE',  ( 0.000000000000000000, 0.000000000000000000, 1.000000000000000000 ) ) ;
#10699 = DIRECTION ( 'NONE',  ( 1.000000000000000000, 0.000000000000000000, 0.000000000000000000 ) ) ;
#10700 = DIRECTION ( 'NONE',  ( 0.000000000000000000, 0.000000000000000000, 1.000000000000000000 ) ) ;
#10701 =( NAMED_UNIT ( * ) SI_UNIT ( $, .STERADIAN. ) SOLID_ANGLE_UNIT ( ) );
#10702 = VECTOR ( 'NONE', #3686, 1000.000000000000114 ) ;
#10703 = CARTESIAN_POINT ( 'NONE',  ( -1.931933921921289571E-14, 6.732211846623371798, -4.339467034331174311 ) ) ;
#10704 = CARTESIAN_POINT ( 'NONE',  ( 198.9111841706756536, 32.15857605477618364, -5.308824953579920347 ) ) ;
#10705 = ORIENTED_EDGE ( 'NONE', *, *, #11020, .T. ) ;
#10706 = CARTESIAN_POINT ( 'NONE',  ( -61.94838851346079167, -181.3058001507315566, 84.88378295107885663 ) ) ;
#10707 = CARTESIAN_POINT ( 'NONE',  ( -221.5581585947747101, 141.9038310245542505, 5.434137442415940988 ) ) ;
#10708 = DIRECTION ( 'NONE',  ( 0.000000000000000000, -0.9902680687415711391, 0.1391731009600603308 ) ) ;
#10709 = DIRECTION ( 'NONE',  ( 0.000000000000000000, 0.000000000000000000, 1.000000000000000000 ) ) ;
#10710 = CARTESIAN_POINT ( 'NONE',  ( 114.0000000000000568, 64.53993994372673626, 13.30000000000035776 ) ) ;
#10711 = VERTEX_POINT ( 'NONE', #1779 ) ;
#10712 = EDGE_LOOP ( 'NONE', ( #7192, #536, #3229 ) ) ;
#10713 = CARTESIAN_POINT ( 'NONE',  ( 177.5000000000000853, 16.03993994372673626, 52.49999999999997868 ) ) ;
#10714 = FACE_OUTER_BOUND ( 'NONE', #15289, .T. ) ;
#10715 = ADVANCED_FACE ( 'NONE', ( #1135 ), #7634, .T. ) ;
#10716 = CIRCLE ( 'NONE', #14224, 3.525000000000000355 ) ;
#10717 = CYLINDRICAL_SURFACE ( 'NONE', #336, 0.5000000000000004441 ) ;
#10718 = DIRECTION ( 'NONE',  ( -1.000000000000000000, 0.000000000000000000, 0.000000000000000000 ) ) ;
#10719 = CARTESIAN_POINT ( 'NONE',  ( -221.3544506110429495, 150.6479677358152856, -4.921649773945601325 ) ) ;
#10720 = CARTESIAN_POINT ( 'NONE',  ( -223.6012825982128902, 142.0449791388664664, 3.334463815293894573 ) ) ;
#10721 = DIRECTION ( 'NONE',  ( 1.000000000000000000, 0.000000000000000000, 0.000000000000000000 ) ) ;
#10722 = DIRECTION ( 'NONE',  ( -1.000000000000000000, 0.000000000000000000, 0.000000000000000000 ) ) ;
#10723 = DIRECTION ( 'NONE',  ( 0.000000000000000000, -1.000000000000000000, -4.956352788505160310E-17 ) ) ;
#10724 = VECTOR ( 'NONE', #10689, 1000.000000000000000 ) ;
#10725 = CARTESIAN_POINT ( 'NONE',  ( 71.96535645333923981, 38.79159067395544014, 5.000000000000000000 ) ) ;
#10726 = CARTESIAN_POINT ( 'NONE',  ( 5.196152422706632024, 9.000000000000003553, 5.000000000000000000 ) ) ;
#10727 = ORIENTED_EDGE ( 'NONE', *, *, #9925, .T. ) ;
#10728 = SHAPE_REPRESENTATION_RELATIONSHIP ( 'NONE' , 'NONE' ,  #7041, #9431 ) ;
#10729 = ORIENTED_EDGE ( 'NONE', *, *, #5051, .F. ) ;
#10730 = EDGE_CURVE ( 'NONE', #12185, #956, #14313, .T. ) ;
#10731 = CARTESIAN_POINT ( 'NONE',  ( 124.2806775638430281, 45.00321902537314145, 0.000000000000000000 ) ) ;
#10732 = DIRECTION ( 'NONE',  ( -0.000000000000000000, 1.000000000000000000, -0.000000000000000000 ) ) ;
#10733 = CARTESIAN_POINT ( 'NONE',  ( -64.00000000000002842, -179.3058001507315566, 84.88378295107887084 ) ) ;
#10734 = CARTESIAN_POINT ( 'NONE',  ( -187.9132138465967898, 138.8208849330412988, 2.500000000000000000 ) ) ;
#10735 = LINE ( 'NONE', #126, #11024 ) ;
#10736 = MANIFOLD_SOLID_BREP ( 'HeadChamfer', #7904 ) ;
#10737 = DIRECTION ( 'NONE',  ( -1.000000000000000000, 0.000000000000000000, 0.000000000000000000 ) ) ;
#10738 = CARTESIAN_POINT ( 'NONE',  ( -206.0222741447286126, 148.9180917377961464, 3.478855109513426580 ) ) ;
#10739 = CIRCLE ( 'NONE', #5439, 1.699999999999993072 ) ;
#10740 = CONICAL_SURFACE ( 'NONE', #5192, 1.219500000000000028, 0.7853981633974552734 ) ;
#10742 = VERTEX_POINT ( 'NONE', #14162 ) ;
#10741 = EDGE_CURVE ( 'NONE', #1584, #13113, #14165, .T. ) ;
#10743 = ADVANCED_BREP_SHAPE_REPRESENTATION ( '', ( #642, #12337 ), #6298 ) ;
#10744 = ORIENTED_EDGE ( 'NONE', *, *, #5991, .T. ) ;
#10745 = CARTESIAN_POINT ( 'NONE',  ( 191.4069380837317453, 39.61051162384328705, -7.503330758807070566 ) ) ;
#10746 = SURFACE_STYLE_FILL_AREA ( #9333 ) ;
#10747 = VERTEX_POINT ( 'NONE', #3592 ) ;
#10748 = CYLINDRICAL_SURFACE ( 'NONE', #6462, 0.5000000000000000000 ) ;
#10749 = CARTESIAN_POINT ( 'NONE',  ( -224.3063355247866468, 145.3592025451120833, 8.356870423832322814 ) ) ;
#10750 = ORIENTED_EDGE ( 'NONE', *, *, #9707, .T. ) ;
#10751 = VERTEX_POINT ( 'NONE', #8199 ) ;
#10752 = CYLINDRICAL_SURFACE ( 'NONE', #1974, 1.700000000000007061 ) ;
#10753 = LINE ( 'NONE', #4827, #2300 ) ;
#10754 = CIRCLE ( 'NONE', #14274, 1.000000000000000888 ) ;
#10755 = EDGE_CURVE ( 'NONE', #379, #15035, #14211, .T. ) ;
#10756 = ORIENTED_EDGE ( 'NONE', *, *, #10307, .T. ) ;
#10757 = CARTESIAN_POINT ( 'NONE',  ( 195.1062858801516597, 40.86394065090267702, 12.00000000000001066 ) ) ;
#10758 = CARTESIAN_POINT ( 'NONE',  ( -70.00000000000000000, 15.53993994372673626, 47.49999999999997868 ) ) ;
#10759 = CARTESIAN_POINT ( 'NONE',  ( -220.3531759299249302, 148.3382346779569616, 2.431557144026069928 ) ) ;
#10760 = MANIFOLD_SOLID_BREP ( 'Cut-Extrude9', #6882 ) ;
#10761 = VERTEX_POINT ( 'NONE', #3435 ) ;
#10762 = CARTESIAN_POINT ( 'NONE',  ( 170.9756796482968184, 59.36285257857151976, -0.9107274384406881529 ) ) ;
#10763 = VERTEX_POINT ( 'NONE', #11733 ) ;
#10764 = EDGE_CURVE ( 'NONE', #12538, #3389, #5728, .T. ) ;
#10765 = CARTESIAN_POINT ( 'NONE',  ( 2.000000000000000000, 1.587713240271468207, -2.750000000000000000 ) ) ;
#10766 = CARTESIAN_POINT ( 'NONE',  ( -192.1704923257120754, 141.1970532186197431, 2.500000000000000000 ) ) ;
#10767 = DIRECTION ( 'NONE',  ( -0.000000000000000000, -6.938893903907227145E-17, 1.000000000000000000 ) ) ;
#10768 = ORIENTED_EDGE ( 'NONE', *, *, #15388, .T. ) ;
#10769 = ORIENTED_EDGE ( 'NONE', *, *, #10806, .T. ) ;
#10770 = CARTESIAN_POINT ( 'NONE',  ( -171.9495551447802200, 125.1641050887067053, -4.702677209512893697 ) ) ;
#10771 = CARTESIAN_POINT ( 'NONE',  ( 201.9353358396146234, 32.56853033914327966, -9.715529407007519325 ) ) ;
#10772 = VERTEX_POINT ( 'NONE', #9367 ) ;
#10773 = EDGE_CURVE ( 'NONE', #8016, #2806, #2718, .T. ) ;
#10774 = ADVANCED_FACE ( 'NONE', ( #324 ), #2805, .F. ) ;
#10775 = CIRCLE ( 'NONE', #5730, 0.5000000000000069944 ) ;
#10776 = DIRECTION ( 'NONE',  ( -1.000000000000000000, 0.000000000000000000, 0.000000000000000000 ) ) ;
#10777 = CARTESIAN_POINT ( 'NONE',  ( 0.000000000000000000, 6.928203230275487456, 4.000000000000003553 ) ) ;
#10778 = EDGE_CURVE ( 'NONE', #11836, #4465, #11409, .T. ) ;
#10779 = CARTESIAN_POINT ( 'NONE',  ( 114.0000000000000568, 62.13993994372673768, 15.00000000000035172 ) ) ;
#10780 = ORIENTED_EDGE ( 'NONE', *, *, #4444, .T. ) ;
#10781 = VECTOR ( 'NONE', #5510, 1000.000000000000000 ) ;
#10782 = CARTESIAN_POINT ( 'NONE',  ( 202.8187013049204950, 32.78779105710274422, -6.518094968334741779 ) ) ;
#10783 = ORIENTED_EDGE ( 'NONE', *, *, #921, .T. ) ;
#10784 = LINE ( 'NONE', #13447, #6352 ) ;
#10785 = CARTESIAN_POINT ( 'NONE',  ( 185.1062858801516882, 55.86394065090267702, 13.00000000000000178 ) ) ;
#10786 = CARTESIAN_POINT ( 'NONE',  ( -199.2256335332332640, 127.9713659812714042, 5.434137442415931218 ) ) ;
#10787 = CARTESIAN_POINT ( 'NONE',  ( 190.5000000000000853, 15.17911304468679745, 25.93769382960994818 ) ) ;
#10788 = ORIENTED_EDGE ( 'NONE', *, *, #4004, .F. ) ;
#10789 = CARTESIAN_POINT ( 'NONE',  ( -198.4250122012724660, 129.4766065029076003, 7.918248976830634334 ) ) ;
#10790 = CARTESIAN_POINT ( 'NONE',  ( -64.00000000000002842, 23.05038067821381986, -0.9395626039331514967 ) ) ;
#10791 = EDGE_CURVE ( 'NONE', #10635, #3817, #4594, .T. ) ;
#10792 = ORIENTED_EDGE ( 'NONE', *, *, #7608, .F. ) ;
#10794 = EDGE_CURVE ( 'NONE', #4995, #2689, #6636, .T. ) ;
#10793 = APPLICATION_CONTEXT ( 'automotive_design' ) ;
#10795 = ORIENTED_EDGE ( 'NONE', *, *, #11550, .T. ) ;
#10796 = CARTESIAN_POINT ( 'NONE',  ( 64.00000000000005684, 59.53993994372674337, 16.70000000000069562 ) ) ;
#10797 = PLANE ( 'NONE',  #11335 ) ;
#10798 = VECTOR ( 'NONE', #10993, 1000.000000000000000 ) ;
#10799 = FACE_OUTER_BOUND ( 'NONE', #9734, .T. ) ;
#10800 = DIRECTION ( 'NONE',  ( -0.4873681696970824651, -0.8731965799097680669, 0.000000000000000000 ) ) ;
#10801 = AXIS2_PLACEMENT_3D ( 'NONE', #4473, #14337, #10647 ) ;
#10802 = DIRECTION ( 'NONE',  ( -0.000000000000000000, -0.000000000000000000, 1.000000000000000000 ) ) ;
#10803 = CARTESIAN_POINT ( 'NONE',  ( 17.41029453487719181, 40.04259805664093363, 10.00000000000000178 ) ) ;
#10804 = DIRECTION ( 'NONE',  ( -0.000000000000000000, 0.000000000000000000, 1.000000000000000000 ) ) ;
#10805 = CARTESIAN_POINT ( 'NONE',  ( -157.4509325786206091, 109.5864172289029881, 9.223488592771900585 ) ) ;
#10806 = EDGE_CURVE ( 'NONE', #649, #3817, #8649, .T. ) ;
#10807 = AXIS2_PLACEMENT_3D ( 'NONE', #8954, #3893, #12556 ) ;
#10808 = DIRECTION ( 'NONE',  ( 0.000000000000000000, -1.000000000000000000, -1.156482317317871478E-16 ) ) ;
#10809 = CARTESIAN_POINT ( 'NONE',  ( 185.1062858801516882, 55.86394065090267702, 13.00000000000000178 ) ) ;
#10810 =( GEOMETRIC_REPRESENTATION_CONTEXT ( 3 ) GLOBAL_UNCERTAINTY_ASSIGNED_CONTEXT ( ( #5206 ) ) GLOBAL_UNIT_ASSIGNED_CONTEXT ( ( #5727, #8267, #4453 ) ) REPRESENTATION_CONTEXT ( 'NONE', 'WORKASPACE' ) );
#10811 = ORIENTED_EDGE ( 'NONE', *, *, #2770, .F. ) ;
#10812 = AXIS2_PLACEMENT_3D ( 'NONE', #1893, #6950, #11757 ) ;
#10813 = ORIENTED_EDGE ( 'NONE', *, *, #11767, .F. ) ;
#10814 = DIRECTION ( 'NONE',  ( -0.000000000000000000, -0.000000000000000000, 1.000000000000000000 ) ) ;
#10815 = CARTESIAN_POINT ( 'NONE',  ( 2.000000000000000000, 1.587713240271470427, 2.750000000000000888 ) ) ;
#10816 = CARTESIAN_POINT ( 'NONE',  ( -85.27455057502459113, 65.19100426474074084, 7.600000000000002309 ) ) ;
#10817 = FACE_OUTER_BOUND ( 'NONE', #7378, .T. ) ;
#10818 = FACE_OUTER_BOUND ( 'NONE', #1726, .T. ) ;
#10819 = MANIFOLD_SOLID_BREP ( 'Mirror1', #3342 ) ;
#10820 = DIRECTION ( 'NONE',  ( 0.000000000000000000, -1.000000000000000000, -1.156482317317871478E-16 ) ) ;
#10821 = CARTESIAN_POINT ( 'NONE',  ( -218.4444600228138711, 155.8616726660956715, 2.500000000270498735 ) ) ;
#10822 = AXIS2_PLACEMENT_3D ( 'NONE', #5118, #1790, #6630 ) ;
#10823 = AXIS2_PLACEMENT_3D ( 'NONE', #5961, #11297, #4030 ) ;
#10824 = ORIENTED_EDGE ( 'NONE', *, *, #8290, .F. ) ;
#10825 = CIRCLE ( 'NONE', #11571, 10.97218105532926558 ) ;
#10826 = ADVANCED_FACE ( 'NONE', ( #14702 ), #6203, .T. ) ;
#10827 = ORIENTED_EDGE ( 'NONE', *, *, #8331, .T. ) ;
#10828 = CARTESIAN_POINT ( 'NONE',  ( 198.9883150731717478, 32.15189384935130334, -6.877829860972676457 ) ) ;
#10829 = EDGE_CURVE ( 'NONE', #4152, #858, #10844, .T. ) ;
#10830 = FILL_AREA_STYLE_COLOUR ( '', #3569 ) ;
#10831 = ORIENTED_EDGE ( 'NONE', *, *, #9435, .F. ) ;
#10832 = CARTESIAN_POINT ( 'NONE',  ( -224.5838421180054070, 144.8620059220666008, 7.877574876664438008 ) ) ;
#10833 = EDGE_LOOP ( 'NONE', ( #6020, #9130, #778, #12230 ) ) ;
#10834 = ORIENTED_EDGE ( 'NONE', *, *, #6731, .T. ) ;
#10835 = FACE_OUTER_BOUND ( 'NONE', #15075, .T. ) ;
#10836 = CARTESIAN_POINT ( 'NONE',  ( 64.00000000000005684, 59.53993994372674337, 13.30000000000070948 ) ) ;
#10837 = VECTOR ( 'NONE', #13833, 1000.000000000000000 ) ;
#10838 = VECTOR ( 'NONE', #1429, 1000.000000000000000 ) ;
#10839 = EDGE_LOOP ( 'NONE', ( #9301, #1981 ) ) ;
#10840 = FACE_OUTER_BOUND ( 'NONE', #6720, .T. ) ;
#10841 = DIRECTION ( 'NONE',  ( -0.000000000000000000, -0.000000000000000000, 1.000000000000000000 ) ) ;
#10842 = AXIS2_PLACEMENT_3D ( 'NONE', #5586, #3130, #10087 ) ;
#10843 = CARTESIAN_POINT ( 'NONE',  ( -110.0000000000000426, 19.53993994372674337, 24.99999999999999645 ) ) ;
#10844 = CIRCLE ( 'NONE', #12090, 7.499999999999999112 ) ;
#10845 = AXIS2_PLACEMENT_3D ( 'NONE', #8248, #5481, #4358 ) ;
#10846 = ORIENTED_EDGE ( 'NONE', *, *, #9050, .F. ) ;
#10847 = CARTESIAN_POINT ( 'NONE',  ( -63.50000000000002842, 15.03993994372673804, 38.07518420361041933 ) ) ;
#10848 = EDGE_CURVE ( 'NONE', #9239, #6280, #165, .T. ) ;
#10849 = LINE ( 'NONE', #4, #5697 ) ;
#10850 = CARTESIAN_POINT ( 'NONE',  ( -222.8347869274849415, 143.8920390286132829, 1.831365460742872209 ) ) ;
#10851 = CARTESIAN_POINT ( 'NONE',  ( 0.000000000000000000, -2.381569860407207084, -1.374999999999997113 ) ) ;
#10852 = VECTOR ( 'NONE', #5426, 1000.000000000000000 ) ;
#10853 = VERTEX_POINT ( 'NONE', #3830 ) ;
#10854 = ORIENTED_EDGE ( 'NONE', *, *, #6610, .F. ) ;
#10855 = CARTESIAN_POINT ( 'NONE',  ( -211.4625087271040513, 151.5689812133889234, -0.4547266291960755935 ) ) ;
#10856 = CARTESIAN_POINT ( 'NONE',  ( 208.8253499713366352, 39.76173270276598970, -9.127040822819912691 ) ) ;
#10857 = VECTOR ( 'NONE', #6594, 1000.000000000000000 ) ;
#10858 = ORIENTED_EDGE ( 'NONE', *, *, #5334, .F. ) ;
#10859 = LINE ( 'NONE', #13038, #3766 ) ;
#10860 = FACE_BOUND ( 'NONE', #7295, .T. ) ;
#10861 = CARTESIAN_POINT ( 'NONE',  ( 167.9295236634097819, 65.51901744756736434, -0.9107274384406985890 ) ) ;
#10862 = AXIS2_PLACEMENT_3D ( 'NONE', #2144, #3177, #10366 ) ;
#10863 = ORIENTED_EDGE ( 'NONE', *, *, #2088, .T. ) ;
#10864 = AXIS2_PLACEMENT_3D ( 'NONE', #15194, #1936, #4388 ) ;
#10865 = ADVANCED_FACE ( 'NONE', ( #2644, #7465, #12259, #1526, #6362, #12801, #7707 ), #15243, .T. ) ;
#10866 = SURFACE_STYLE_FILL_AREA ( #9598 ) ;
#10867 = CARTESIAN_POINT ( 'NONE',  ( 205.5168546899054434, 47.82311440310952833, -1.064259200291542529 ) ) ;
#10868 = EDGE_LOOP ( 'NONE', ( #14082, #13975, #12953, #8480 ) ) ;
#10869 = FACE_OUTER_BOUND ( 'NONE', #11217, .T. ) ;
#10870 = CARTESIAN_POINT ( 'NONE',  ( -110.0000000000000426, 19.53993994372674337, 9.999999999999998224 ) ) ;
#10871 = CARTESIAN_POINT ( 'NONE',  ( -209.2398179475638926, 133.3202902034983595, 5.434137442415948094 ) ) ;
#10872 = DIRECTION ( 'NONE',  ( 0.000000000000000000, 0.000000000000000000, -1.000000000000000000 ) ) ;
#10873 = ORIENTED_EDGE ( 'NONE', *, *, #1736, .F. ) ;
#10874 = CARTESIAN_POINT ( 'NONE',  ( -189.6066827460468858, 129.2255495722319836, 9.577123744044220288 ) ) ;
#10875 = CYLINDRICAL_SURFACE ( 'NONE', #10120, 0.5000000000000001110 ) ;
#10876 = ORIENTED_EDGE ( 'NONE', *, *, #7793, .F. ) ;
#10877 = ORIENTED_EDGE ( 'NONE', *, *, #14236, .F. ) ;
#10878 = AXIS2_PLACEMENT_3D ( 'NONE', #11455, #539, #4175 ) ;
#10879 = CARTESIAN_POINT ( 'NONE',  ( -194.4336556300434893, 127.2574632897803326, 2.431555724346868175 ) ) ;
#10880 = CARTESIAN_POINT ( 'NONE',  ( 0.3194001229790260354, 3.115132258388565223, -7.999999999999979572 ) ) ;
#10881 = CIRCLE ( 'NONE', #4050, 2.749999999999999112 ) ;
#10882 = CARTESIAN_POINT ( 'NONE',  ( -76.00000000000001421, 15.17911304468679923, 9.062306170389897275 ) ) ;
#10883 = DIRECTION ( 'NONE',  ( -0.000000000000000000, -0.000000000000000000, 1.000000000000000000 ) ) ;
#10884 = CARTESIAN_POINT ( 'NONE',  ( -225.6712625649270478, 142.9137214952622514, 1.583163137451349511 ) ) ;
#10885 = CARTESIAN_POINT ( 'NONE',  ( -222.4620031969695049, 144.3197956335804122, 8.205567776478527975 ) ) ;
#10886 = EDGE_CURVE ( 'NONE', #7691, #1354, #4273, .T. ) ;
#10887 = EDGE_CURVE ( 'NONE', #5154, #8651, #9573, .T. ) ;
#10888 = EDGE_CURVE ( 'NONE', #2654, #12864, #7576, .T. ) ;
#10889 = FACE_OUTER_BOUND ( 'NONE', #7174, .T. ) ;
#10890 = VECTOR ( 'NONE', #10732, 1000.000000000000000 ) ;
#10891 = DIRECTION ( 'NONE',  ( -1.000000000000000000, 0.000000000000000000, 0.000000000000000000 ) ) ;
#10892 = LINE ( 'NONE', #11117, #12300 ) ;
#10893 = VECTOR ( 'NONE', #14546, 1000.000000000000000 ) ;
#10894 = CARTESIAN_POINT ( 'NONE',  ( -70.00000000000000000, 15.53993994372673981, -13.99999999999999112 ) ) ;
#10895 = VERTEX_POINT ( 'NONE', #13921 ) ;
#10896 = VERTEX_POINT ( 'NONE', #15167 ) ;
#10897 = CARTESIAN_POINT ( 'NONE',  ( 0.000000000000000000, 0.000000000000000000, 0.000000000000000000 ) ) ;
#10898 = DIRECTION ( 'NONE',  ( 0.4873681696970831312, 0.8731965799097676229, 0.000000000000000000 ) ) ;
#10899 = CYLINDRICAL_SURFACE ( 'NONE', #2840, 1.700000000000001954 ) ;
#10900 = CARTESIAN_POINT ( 'NONE',  ( 7.890111903673804700E-16, 0.2688604483224075747, 2.750000000000000888 ) ) ;
#10901 = AXIS2_PLACEMENT_3D ( 'NONE', #1472, #8681, #13475 ) ;
#10902 = FACE_OUTER_BOUND ( 'NONE', #12080, .T. ) ;
#10903 = DIRECTION ( 'NONE',  ( -1.000000000000000000, 0.000000000000000000, 0.000000000000000000 ) ) ;
#10904 = ADVANCED_FACE ( 'NONE', ( #4438 ), #1837, .F. ) ;
#10905 = MECHANICAL_DESIGN_GEOMETRIC_PRESENTATION_REPRESENTATION (  '', ( #5592 ), #13920 ) ;
#10906 = EDGE_LOOP ( 'NONE', ( #7829, #1410, #7813, #12179 ) ) ;
#10907 = ORIENTED_EDGE ( 'NONE', *, *, #14756, .T. ) ;
#10908 = CARTESIAN_POINT ( 'NONE',  ( 194.8335778941103626, 33.83376941343732369, -4.128887708184892702 ) ) ;
#10909 = CARTESIAN_POINT ( 'NONE',  ( -63.50000000000002842, -178.8058001507315566, -17.19066787724516843 ) ) ;
#10910 = ORIENTED_EDGE ( 'NONE', *, *, #3279, .F. ) ;
#10911 = STYLED_ITEM ( 'NONE', ( #11809 ), #10760 ) ;
#10912 = CARTESIAN_POINT ( 'NONE',  ( -223.0117914826104766, 143.2331855431448560, 6.837811219071827651 ) ) ;
#10913 = ORIENTED_EDGE ( 'NONE', *, *, #11149, .T. ) ;
#10914 = LINE ( 'NONE', #14366, #3008 ) ;
#10915 = CIRCLE ( 'NONE', #5866, 1.700000000000007061 ) ;
#10916 = CARTESIAN_POINT ( 'NONE',  ( 202.6027916890166694, 29.64969172180087398, -8.171549047034778468 ) ) ;
#10917 = ORIENTED_EDGE ( 'NONE', *, *, #15166, .F. ) ;
#10918 = CARTESIAN_POINT ( 'NONE',  ( -61.94838851346079167, 15.03993994372673981, -3.075184203610571654 ) ) ;
#10919 = DIRECTION ( 'NONE',  ( 0.000000000000000000, 1.000000000000000000, 6.938893903907227145E-17 ) ) ;
#10920 = EDGE_CURVE ( 'NONE', #4028, #12308, #719, .T. ) ;
#10921 = EDGE_CURVE ( 'NONE', #4524, #1269, #1756, .T. ) ;
#10922 = CARTESIAN_POINT ( 'NONE',  ( 2.000000000000000000, 3.175426480542944407, 0.000000000000000000 ) ) ;
#10923 = AXIS2_PLACEMENT_3D ( 'NONE', #8775, #12396, #10121 ) ;
#10924 = ORIENTED_EDGE ( 'NONE', *, *, #5935, .F. ) ;
#10925 = CARTESIAN_POINT ( 'NONE',  ( 70.26535645333922275, 38.79159067395544014, 10.00000000000000178 ) ) ;
#10926 = ORIENTED_EDGE ( 'NONE', *, *, #13091, .F. ) ;
#10927 = CIRCLE ( 'NONE', #14967, 0.5000000000000004441 ) ;
#10928 = DIRECTION ( 'NONE',  ( 0.000000000000000000, 0.000000000000000000, -1.000000000000000000 ) ) ;
#10929 = DIRECTION ( 'NONE',  ( -0.000000000000000000, -0.000000000000000000, 1.000000000000000000 ) ) ;
#10930 = ORIENTED_EDGE ( 'NONE', *, *, #12087, .T. ) ;
#10931 = EDGE_LOOP ( 'NONE', ( #4625, #13011, #1728, #11008, #5813 ) ) ;
#10932 = CARTESIAN_POINT ( 'NONE',  ( -202.0520865685784884, 146.2723300204251018, -0.4547266291960743168 ) ) ;
#10933 = CARTESIAN_POINT ( 'NONE',  ( 188.2949840871649485, 42.33905491644829766, -4.631930676406226688 ) ) ;
#10934 = ORIENTED_EDGE ( 'NONE', *, *, #1926, .T. ) ;
#10935 = EDGE_CURVE ( 'NONE', #10667, #4671, #14606, .T. ) ;
#10936 = AXIS2_PLACEMENT_3D ( 'NONE', #6865, #4471, #9157 ) ;
#10937 = CARTESIAN_POINT ( 'NONE',  ( 66.74035645333923128, 38.79159067395544014, 10.00000000000000178 ) ) ;
#10938 = DIRECTION ( 'NONE',  ( 0.000000000000000000, 1.000000000000000000, 0.000000000000000000 ) ) ;
#10939 = DIRECTION ( 'NONE',  ( -0.000000000000000000, -0.000000000000000000, 1.000000000000000000 ) ) ;
#10940 = ORIENTED_EDGE ( 'NONE', *, *, #12915, .T. ) ;
#10941 = ADVANCED_FACE ( 'NONE', ( #6827 ), #9197, .T. ) ;
#10942 = DIRECTION ( 'NONE',  ( 0.000000000000000000, -1.000000000000000000, -1.156482317317871725E-16 ) ) ;
#10943 = CARTESIAN_POINT ( 'NONE',  ( 207.3546231538492179, 50.29643094772573164, -2.498001438440778710 ) ) ;
#10944 = ORIENTED_EDGE ( 'NONE', *, *, #9810, .F. ) ;
#10945 = CARTESIAN_POINT ( 'NONE',  ( -64.00000000000002842, -178.8058001507315566, 65.31842631998698323 ) ) ;
#10946 = DIRECTION ( 'NONE',  ( 0.000000000000000000, 0.1391731009600660485, -0.9902680687415702510 ) ) ;
#10947 = AXIS2_PLACEMENT_3D ( 'NONE', #8669, #2588, #10081 ) ;
#10948 = CARTESIAN_POINT ( 'NONE',  ( -217.9771163551940276, 139.5700662992579737, 5.434137442415948982 ) ) ;
#10949 = ADVANCED_FACE ( 'NONE', ( #15089 ), #9327, .T. ) ;
#10950 = DIRECTION ( 'NONE',  ( 0.000000000000000000, -0.8660254037844379305, 0.5000000000000012212 ) ) ;
#10951 = ORIENTED_EDGE ( 'NONE', *, *, #9909, .F. ) ;
#10952 = CARTESIAN_POINT ( 'NONE',  ( -198.9139648670198994, 132.3922632189928095, 9.577123744044227394 ) ) ;
#10953 = DIRECTION ( 'NONE',  ( 8.659560562354932858E-17, 0.7071067811865474617, -0.7071067811865474617 ) ) ;
#10954 = ORIENTED_EDGE ( 'NONE', *, *, #2433, .F. ) ;
#10955 = ORIENTED_EDGE ( 'NONE', *, *, #8384, .T. ) ;
#10956 = CARTESIAN_POINT ( 'NONE',  ( 5.799999999999999822, 6.928203230275514990, -4.000000000000003553 ) ) ;
#10957 = DIRECTION ( 'NONE',  ( 0.000000000000000000, 0.000000000000000000, 1.000000000000000000 ) ) ;
#10958 = EDGE_CURVE ( 'NONE', #4614, #12779, #13994, .T. ) ;
#10959 = DIRECTION ( 'NONE',  ( 0.000000000000000000, 0.000000000000000000, 1.000000000000000000 ) ) ;
#10960 = DIRECTION ( 'NONE',  ( 0.000000000000000000, -1.000000000000000000, 0.000000000000000000 ) ) ;
#10961 = CARTESIAN_POINT ( 'NONE',  ( 184.0000000000000568, 15.53993994372673981, -13.99999999999999112 ) ) ;
#10962 = AXIS2_PLACEMENT_3D ( 'NONE', #4724, #14662, #1474 ) ;
#10963 = CYLINDRICAL_SURFACE ( 'NONE', #4633, 5.000000000000004441 ) ;
#10964 = CARTESIAN_POINT ( 'NONE',  ( -156.7621818139058405, 109.1948612100107994, 9.220837571243208686 ) ) ;
#10965 = DIRECTION ( 'NONE',  ( -0.000000000000000000, 1.000000000000000000, -0.000000000000000000 ) ) ;
#10966 = CARTESIAN_POINT ( 'NONE',  ( 178.0000000000000853, -179.3058001507315566, -17.76585208085566947 ) ) ;
#10967 = CARTESIAN_POINT ( 'NONE',  ( 169.0043059057019832, 61.25683321636181233, 10.00000000000000178 ) ) ;
#10968 = ORIENTED_EDGE ( 'NONE', *, *, #11334, .F. ) ;
#10969 = EDGE_CURVE ( 'NONE', #1214, #8453, #2000, .T. ) ;
#10970 = AXIS2_PLACEMENT_3D ( 'NONE', #12115, #4777, #11890 ) ;
#10971 = VERTEX_POINT ( 'NONE', #1914 ) ;
#10972 = DIRECTION ( 'NONE',  ( 1.000000000000000000, 0.000000000000000000, 0.000000000000000000 ) ) ;
#10973 = CARTESIAN_POINT ( 'NONE',  ( -76.00000000000001421, -179.3058001507315566, -51.45141194869120937 ) ) ;
#10974 = FACE_BOUND ( 'NONE', #8551, .T. ) ;
#10976 = EDGE_CURVE ( 'NONE', #5209, #13055, #3111, .T. ) ;
#10975 = EDGE_CURVE ( 'NONE', #5430, #14943, #5319, .T. ) ;
#10977 = EDGE_CURVE ( 'NONE', #13329, #11305, #4527, .T. ) ;
#10978 = CARTESIAN_POINT ( 'NONE',  ( 0.000000000000000000, 0.000000000000000000, 0.000000000000000000 ) ) ;
#10979 = CARTESIAN_POINT ( 'NONE',  ( -206.8718859864436581, 149.4025266312245037, 2.500000000000000000 ) ) ;
#10980 = ADVANCED_FACE ( 'NONE', ( #13759 ), #1761, .T. ) ;
#10981 = ORIENTED_EDGE ( 'NONE', *, *, #15191, .F. ) ;
#10982 = ORIENTED_EDGE ( 'NONE', *, *, #9453, .F. ) ;
#10983 = CARTESIAN_POINT ( 'NONE',  ( 201.3303440367248243, 32.15585396293944598, -6.755036635249508592 ) ) ;
#10984 = DIRECTION ( 'NONE',  ( 1.000000000000000000, 0.000000000000000000, 0.000000000000000000 ) ) ;
#10985 = VERTEX_POINT ( 'NONE', #10296 ) ;
#10986 = CARTESIAN_POINT ( 'NONE',  ( -223.0208697908820739, 147.6623161915171636, 9.682315826541753268 ) ) ;
#10987 = ORIENTED_EDGE ( 'NONE', *, *, #6979, .F. ) ;
#10988 = DIRECTION ( 'NONE',  ( -0.5000000000000001110, 0.8660254037844385966, 0.000000000000000000 ) ) ;
#10989 = CARTESIAN_POINT ( 'NONE',  ( 211.8984647248233273, 39.28052202550077965, -7.564127153369329726 ) ) ;
#10990 = CIRCLE ( 'NONE', #4945, 1.700000000000000178 ) ;
#10991 = ADVANCED_FACE ( 'NONE', ( #4278, #8178 ), #11946, .T. ) ;
#10992 = ORIENTED_EDGE ( 'NONE', *, *, #4277, .T. ) ;
#10993 = DIRECTION ( 'NONE',  ( -0.000000000000000000, 1.000000000000000000, 1.156482317317871725E-16 ) ) ;
#10994 = CARTESIAN_POINT ( 'NONE',  ( 177.5000000000000853, -178.9449732516916072, 64.32815825124541220 ) ) ;
#10995 = CIRCLE ( 'NONE', #2671, 3.525000000000000355 ) ;
#10996 = CARTESIAN_POINT ( 'NONE',  ( 163.3793289068652257, 15.80605437029538507, -6.370175303308196924 ) ) ;
#10997 = ORIENTED_EDGE ( 'NONE', *, *, #12547, .F. ) ;
#10998 = EDGE_LOOP ( 'NONE', ( #11429, #8932, #8853, #15528 ) ) ;
#10999 = CARTESIAN_POINT ( 'NONE',  ( 186.1005832062958234, 72.46888774096882457, 10.00000000000000178 ) ) ;
#11000 = ORIENTED_EDGE ( 'NONE', *, *, #10829, .F. ) ;
#11001 = CARTESIAN_POINT ( 'NONE',  ( 114.0000000000000426, 15.53993994372673981, 7.305634244248866343E-16 ) ) ;
#11002 = EDGE_CURVE ( 'NONE', #12934, #3554, #13342, .T. ) ;
#11003 = CARTESIAN_POINT ( 'NONE',  ( -150.4086188282879277, 107.2728346664360259, -4.856732557889654522 ) ) ;
#11004 = EDGE_LOOP ( 'NONE', ( #9656, #1 ) ) ;
#11005 = ORIENTED_EDGE ( 'NONE', *, *, #1850, .T. ) ;
#11006 = CARTESIAN_POINT ( 'NONE',  ( -177.5434268683390826, 132.5922366007948199, -0.4547266291960713747 ) ) ;
#11007 = CARTESIAN_POINT ( 'NONE',  ( 191.3918663844754349, 39.68659111044760124, -5.934329888686073140 ) ) ;
#11008 = ORIENTED_EDGE ( 'NONE', *, *, #8157, .T. ) ;
#11009 = CARTESIAN_POINT ( 'NONE',  ( -38.29899788034579444, 48.72489408690345414, 7.600000000000002309 ) ) ;
#11010 = DIRECTION ( 'NONE',  ( 0.4873681696970812438, 0.8731965799097687331, -0.000000000000000000 ) ) ;
#11011 = AXIS2_PLACEMENT_3D ( 'NONE', #14582, #7273, #15527 ) ;
#11012 = DIRECTION ( 'NONE',  ( -0.7900120431063429871, 0.6130913241491365850, 0.000000000000000000 ) ) ;
#11013 = AXIS2_PLACEMENT_3D ( 'NONE', #6065, #10883, #38 ) ;
#11014 = ORIENTED_EDGE ( 'NONE', *, *, #14625, .T. ) ;
#11015 = CARTESIAN_POINT ( 'NONE',  ( 192.8460887339186343, 31.43990810023382920, -3.998601258139535819 ) ) ;
#11016 = ORIENTED_EDGE ( 'NONE', *, *, #11440, .F. ) ;
#11017 = DIRECTION ( 'NONE',  ( 1.000000000000000000, 0.000000000000000000, 0.000000000000000000 ) ) ;
#11018 = LINE ( 'NONE', #13371, #878 ) ;
#11019 = CARTESIAN_POINT ( 'NONE',  ( -177.2366359034146512, 121.3924996022181375, -4.733667549831950261 ) ) ;
#11020 = EDGE_CURVE ( 'NONE', #3704, #234, #3490, .T. ) ;
#11021 = DIRECTION ( 'NONE',  ( 0.000000000000000000, 0.000000000000000000, -1.000000000000000000 ) ) ;
#11022 = ORIENTED_EDGE ( 'NONE', *, *, #14756, .F. ) ;
#11023 = CARTESIAN_POINT ( 'NONE',  ( -223.5464781713420734, 146.7206062712571111, 9.530069280832668355 ) ) ;
#11024 = VECTOR ( 'NONE', #8382, 1000.000000000000000 ) ;
#11025 = CARTESIAN_POINT ( 'NONE',  ( 208.8313558426846157, 41.97310978343666932, 0.1351797820921298021 ) ) ;
#11026 = VERTEX_POINT ( 'NONE', #10522 ) ;
#11027 = ORIENTED_EDGE ( 'NONE', *, *, #5991, .F. ) ;
#11028 = DIRECTION ( 'NONE',  ( -0.000000000000000000, 0.000000000000000000, 1.000000000000000000 ) ) ;
#11029 = DIRECTION ( 'NONE',  ( 0.000000000000000000, 0.000000000000000000, -1.000000000000000000 ) ) ;
#11030 = FACE_OUTER_BOUND ( 'NONE', #724, .T. ) ;
#11031 = DIRECTION ( 'NONE',  ( 0.000000000000000000, 0.9902680687415712502, 0.1391731009600586100 ) ) ;
#11032 = LINE ( 'NONE', #9859, #2391 ) ;
#11033 = EDGE_CURVE ( 'NONE', #5777, #13203, #12583, .T. ) ;
#11034 = DIRECTION ( 'NONE',  ( 3.965082230804130220E-16, 4.956352788505162775E-17, -1.000000000000000000 ) ) ;
#11035 = CARTESIAN_POINT ( 'NONE',  ( 184.0000000000000568, 15.53993994372673981, -12.49999999999999289 ) ) ;
#11036 = ORIENTED_EDGE ( 'NONE', *, *, #6650, .T. ) ;
#11037 = EDGE_CURVE ( 'NONE', #1785, #6229, #8077, .T. ) ;
#11038 = FACE_OUTER_BOUND ( 'NONE', #8874, .T. ) ;
#11039 = AXIS2_PLACEMENT_3D ( 'NONE', #3313, #6954, #9317 ) ;
#11040 = ORIENTED_EDGE ( 'NONE', *, *, #6696, .T. ) ;
#11041 = LINE ( 'NONE', #9868, #692 ) ;
#11042 = LINE ( 'NONE', #10973, #5841 ) ;
#11043 = AXIS2_PLACEMENT_3D ( 'NONE', #4259, #14417, #3539 ) ;
#11044 = CARTESIAN_POINT ( 'NONE',  ( 190.0000000000000568, -178.8058001507315566, 52.19066787724494816 ) ) ;
#11045 = CARTESIAN_POINT ( 'NONE',  ( 184.0000000000000568, -181.3058001507315566, 74.95141194869098911 ) ) ;
#11046 = DIRECTION ( 'NONE',  ( 0.000000000000000000, -0.8660254037844382635, -0.5000000000000006661 ) ) ;
#11047 = LINE ( 'NONE', #2522, #15354 ) ;
#11048 = CARTESIAN_POINT ( 'NONE',  ( -187.9132138465967898, 138.8208849330412988, 2.500000000000000000 ) ) ;
#11050 = ORIENTED_EDGE ( 'NONE', *, *, #1187, .F. ) ;
#11049 = EDGE_CURVE ( 'NONE', #10652, #11836, #1118, .T. ) ;
#11051 = VECTOR ( 'NONE', #10173, 1000.000000000000000 ) ;
#11052 = DIRECTION ( 'NONE',  ( 0.000000000000000000, 0.000000000000000000, -1.000000000000000000 ) ) ;
#11053 = EDGE_CURVE ( 'NONE', #720, #831, #14220, .T. ) ;
#11054 = CARTESIAN_POINT ( 'NONE',  ( 201.2368453335255936, 49.57344380111126725, -8.378533376203868954 ) ) ;
#11055 = CARTESIAN_POINT ( 'NONE',  ( 5.799999999999999822, 4.618802153516981868, -7.999999999999979572 ) ) ;
#11056 = ORIENTED_EDGE ( 'NONE', *, *, #1604, .T. ) ;
#11057 = EDGE_CURVE ( 'NONE', #4694, #3509, #11869, .T. ) ;
#11058 = CARTESIAN_POINT ( 'NONE',  ( -223.5526519068884852, 142.1455622009127637, 3.981868244017999992 ) ) ;
#11059 = VERTEX_POINT ( 'NONE', #10762 ) ;
#11060 = ADVANCED_FACE ( 'NONE', ( #5712 ), #9841, .T. ) ;
#11061 = CARTESIAN_POINT ( 'NONE',  ( -173.0510230909240192, 118.1845996390716351, -3.619230586480127076 ) ) ;
#11062 = CARTESIAN_POINT ( 'NONE',  ( 188.3116205180919565, 39.28179296801131670, -5.943714943518696003 ) ) ;
#11063 = ORIENTED_EDGE ( 'NONE', *, *, #13225, .T. ) ;
#11064 = CARTESIAN_POINT ( 'NONE',  ( -63.50000000000002842, 17.53993994372673981, -17.50000000000002487 ) ) ;
#11065 = LINE ( 'NONE', #217, #9862 ) ;
#11066 = AXIS2_PLACEMENT_3D ( 'NONE', #15182, #6498, #13576 ) ;
#11067 = AXIS2_PLACEMENT_3D ( 'NONE', #171, #5019, #13213 ) ;
#11068 = DIRECTION ( 'NONE',  ( 3.965082230804130220E-16, 1.486905836551548832E-16, -1.000000000000000000 ) ) ;
#11069 = ORIENTED_EDGE ( 'NONE', *, *, #12648, .F. ) ;
#11070 = MANIFOLD_SOLID_BREP ( 'Fillet4', #9397 ) ;
#11071 = VERTEX_POINT ( 'NONE', #6022 ) ;
#11072 = EDGE_CURVE ( 'NONE', #1807, #13446, #15602, .T. ) ;
#11073 = ADVANCED_FACE ( 'NONE', ( #8101 ), #12886, .F. ) ;
#11074 = CARTESIAN_POINT ( 'NONE',  ( 178.0000000000000853, 16.03993994372673981, 38.07518420361041933 ) ) ;
#11075 = EDGE_CURVE ( 'NONE', #15428, #899, #12245, .T. ) ;
#11076 = VECTOR ( 'NONE', #3152, 1000.000000000000000 ) ;
#11077 = ORIENTED_EDGE ( 'NONE', *, *, #4140, .F. ) ;
#11079 = VECTOR ( 'NONE', #14628, 1000.000000000000000 ) ;
#11078 = CARTESIAN_POINT ( 'NONE',  ( -5.196152422706636465, 9.000000000000001776, 0.000000000000000000 ) ) ;
#11080 = CYLINDRICAL_SURFACE ( 'NONE', #6040, 1.499999999999995115 ) ;
#11081 = ORIENTED_EDGE ( 'NONE', *, *, #4214, .F. ) ;
#11082 = ORIENTED_EDGE ( 'NONE', *, *, #13719, .F. ) ;
#11083 = DIRECTION ( 'NONE',  ( -0.4999999999999999445, 0.8660254037844385966, 0.000000000000000000 ) ) ;
#11084 = CARTESIAN_POINT ( 'NONE',  ( 208.8051451104704768, 39.65587490144260840, -4.559632177755815086 ) ) ;
#11085 = VERTEX_POINT ( 'NONE', #6343 ) ;
#11086 = DIRECTION ( 'NONE',  ( -1.000000000000000000, 0.000000000000000000, 0.000000000000000000 ) ) ;
#11087 = LINE ( 'NONE', #2639, #11496 ) ;
#11088 = CIRCLE ( 'NONE', #4257, 0.5000000000000004441 ) ;
#11089 = DIRECTION ( 'NONE',  ( 0.000000000000000000, -0.1391731009600660485, -0.9902680687415702510 ) ) ;
#11090 = AXIS2_PLACEMENT_3D ( 'NONE', #13278, #6274, #12106 ) ;
#11091 = EDGE_CURVE ( 'NONE', #12980, #1879, #5071, .T. ) ;
#11092 = CARTESIAN_POINT ( 'NONE',  ( 178.0000000000000853, 15.17911304468680100, 9.062306170389884841 ) ) ;
#11093 = AXIS2_PLACEMENT_3D ( 'NONE', #8039, #3367, #7005 ) ;
#11094 = CARTESIAN_POINT ( 'NONE',  ( 201.8058794277662571, 52.63602710067958412, -5.247041060177010330 ) ) ;
#11095 = ORIENTED_EDGE ( 'NONE', *, *, #11728, .T. ) ;
#11096 = DIRECTION ( 'NONE',  ( 1.000000000000000000, 2.751328491981765035E-32, -3.965082230804130220E-16 ) ) ;
#11097 = FACE_OUTER_BOUND ( 'NONE', #7131, .T. ) ;
#11098 = VECTOR ( 'NONE', #6259, 1000.000000000000000 ) ;
#11099 = CARTESIAN_POINT ( 'NONE',  ( -213.3556830655219585, 148.0789703896194567, -4.640918829492433950 ) ) ;
#11100 = VECTOR ( 'NONE', #8607, 1000.000000000000000 ) ;
#11101 = CYLINDRICAL_SURFACE ( 'NONE', #1980, 1.000000000000000888 ) ;
#11102 = ORIENTED_EDGE ( 'NONE', *, *, #2246, .T. ) ;
#11103 = CARTESIAN_POINT ( 'NONE',  ( -174.5069932933876942, 126.2863744793834826, 9.536681319450917016 ) ) ;
#11104 = AXIS2_PLACEMENT_3D ( 'NONE', #12721, #6980, #3257 ) ;
#11105 = CARTESIAN_POINT ( 'NONE',  ( 191.4322133549729585, 42.19665789901188901, -4.493471110936619439 ) ) ;
#11106 = MANIFOLD_SOLID_BREP ( 'Cut-Extrude4', #14647 ) ;
#11107 = VERTEX_POINT ( 'NONE', #7607 ) ;
#11108 = ORIENTED_EDGE ( 'NONE', *, *, #14841, .F. ) ;
#11109 = DIRECTION ( 'NONE',  ( 0.000000000000000000, 0.000000000000000000, 1.000000000000000000 ) ) ;
#11110 = DIRECTION ( 'NONE',  ( 0.000000000000000000, 0.000000000000000000, 1.000000000000000000 ) ) ;
#11111 = EDGE_CURVE ( 'NONE', #627, #9960, #13206, .T. ) ;
#11112 = CIRCLE ( 'NONE', #3787, 7.499999999999999112 ) ;
#11113 = CARTESIAN_POINT ( 'NONE',  ( 70.26535645333922275, 38.79159067395544014, 9.975000000000001421 ) ) ;
#11114 = CARTESIAN_POINT ( 'NONE',  ( -63.50000000000002842, 15.60952649420677041, 9.122796835852554409 ) ) ;
#11115 = CARTESIAN_POINT ( 'NONE',  ( 0.09566599640799457183, 1.847441354476763165, 2.300137710042383432 ) ) ;
#11116 = CARTESIAN_POINT ( 'NONE',  ( -198.7725242955204692, 144.3921638819772113, 5.434754235172606585 ) ) ;
#11117 = CARTESIAN_POINT ( 'NONE',  ( -76.50000000000004263, 17.53993994372673271, 52.49999999999997868 ) ) ;
#11118 = VECTOR ( 'NONE', #6574, 1000.000000000000000 ) ;
#11119 = DIRECTION ( 'NONE',  ( 0.9296197478520974444, 0.3660421972118351741, -0.04266420354037655377 ) ) ;
#11120 = ORIENTED_EDGE ( 'NONE', *, *, #11530, .F. ) ;
#11122 = CARTESIAN_POINT ( 'NONE',  ( 14.00000000000004086, 59.53993994372674337, 13.30000000000105231 ) ) ;
#11121 = VECTOR ( 'NONE', #5663, 1000.000000000000114 ) ;
#11123 = ORIENTED_EDGE ( 'NONE', *, *, #2169, .T. ) ;
#11124 = ADVANCED_FACE ( 'NONE', ( #8482 ), #14610, .T. ) ;
#11125 = EDGE_LOOP ( 'NONE', ( #12753, #2919, #1570, #3205 ) ) ;
#11126 = FACE_OUTER_BOUND ( 'NONE', #8464, .T. ) ;
#11127 = DIRECTION ( 'NONE',  ( -0.000000000000000000, 1.000000000000000000, 1.156482317317871725E-16 ) ) ;
#11128 = CARTESIAN_POINT ( 'NONE',  ( 177.5000000000000853, 15.03993994372673981, 10.05257423913146475 ) ) ;
#11129 = DIRECTION ( 'NONE',  ( 0.000000000000000000, 0.000000000000000000, 1.000000000000000000 ) ) ;
#11130 = CARTESIAN_POINT ( 'NONE',  ( 114.0000000000000426, 15.53993994372673981, 7.305634244248866343E-16 ) ) ;
#11131 = CARTESIAN_POINT ( 'NONE',  ( -9.724672249307026221E-16, -2.111069397712039830, -1.843520544858919807 ) ) ;
#11132 = CARTESIAN_POINT ( 'NONE',  ( -178.4232521731099439, 131.0169814278324907, 7.919662025281895446 ) ) ;
#11133 = ORIENTED_EDGE ( 'NONE', *, *, #12307, .F. ) ;
#11134 = AXIS2_PLACEMENT_3D ( 'NONE', #2492, #2414, #9524 ) ;
#11135 = AXIS2_PLACEMENT_3D ( 'NONE', #7043, #15383, #13015 ) ;
#11136 = ADVANCED_FACE ( 'NONE', ( #13346 ), #8629, .F. ) ;
#11137 = CARTESIAN_POINT ( 'NONE',  ( 208.8162124854775357, 42.04914431719598156, -1.433821094984975009 ) ) ;
#11138 = CARTESIAN_POINT ( 'NONE',  ( -224.2481407916400542, 145.4634675445406913, 5.252818170846536461 ) ) ;
#11139 = ORIENTED_EDGE ( 'NONE', *, *, #3369, .T. ) ;
#11140 = CARTESIAN_POINT ( 'NONE',  ( -220.4524996695633092, 148.1714595847825819, 9.941101666187114105 ) ) ;
#11141 = ORIENTED_EDGE ( 'NONE', *, *, #9778, .F. ) ;
#11142 = FACE_OUTER_BOUND ( 'NONE', #11523, .T. ) ;
#11143 = CARTESIAN_POINT ( 'NONE',  ( 207.4378898283430885, 50.27467837972982068, -1.073754539701174959 ) ) ;
#11144 = AXIS2_PLACEMENT_3D ( 'NONE', #12537, #10113, #5530 ) ;
#11145 = ORIENTED_EDGE ( 'NONE', *, *, #4111, .F. ) ;
#11146 = DIRECTION ( 'NONE',  ( -1.000000000000000000, 0.000000000000000000, 0.000000000000000000 ) ) ;
#11147 = CYLINDRICAL_SURFACE ( 'NONE', #6587, 1.699999999999991518 ) ;
#11148 = TOROIDAL_SURFACE ( 'NONE', #7377, 1.000000000000000000, 0.5000000000000000000 ) ;
#11149 = EDGE_CURVE ( 'NONE', #299, #14837, #2627, .T. ) ;
#11150 = CARTESIAN_POINT ( 'NONE',  ( 70.26535645333922275, 38.79159067395544014, 10.00000000000000178 ) ) ;
#11151 = VERTEX_POINT ( 'NONE', #6423 ) ;
#11152 = AXIS2_PLACEMENT_3D ( 'NONE', #12665, #6765, #12822 ) ;
#11153 = VERTEX_POINT ( 'NONE', #12169 ) ;
#11154 = FACE_OUTER_BOUND ( 'NONE', #8184, .T. ) ;
#11155 = CIRCLE ( 'NONE', #8401, 3.500000000000004885 ) ;
#11156 = DIRECTION ( 'NONE',  ( -0.3663757939738424008, 0.9304669674900000187, 0.000000000000000000 ) ) ;
#11157 = VERTEX_POINT ( 'NONE', #1271 ) ;
#11158 = LINE ( 'NONE', #311, #1896 ) ;
#11159 = DIRECTION ( 'NONE',  ( -0.000000000000000000, -0.000000000000000000, 1.000000000000000000 ) ) ;
#11160 = ORIENTED_EDGE ( 'NONE', *, *, #9412, .F. ) ;
#11161 = ORIENTED_EDGE ( 'NONE', *, *, #6028, .F. ) ;
#11162 = CARTESIAN_POINT ( 'NONE',  ( -211.2987210398670186, 151.8733316563206586, 2.500000000000000000 ) ) ;
#11163 = CARTESIAN_POINT ( 'NONE',  ( 207.0699012803337951, 46.20241706079673349, -2.754725152881798866 ) ) ;
#11164 = ORIENTED_EDGE ( 'NONE', *, *, #13060, .F. ) ;
#11165 = CARTESIAN_POINT ( 'NONE',  ( 190.5000000000000853, 15.60952649420676686, 25.87720316414728217 ) ) ;
#11166 = CARTESIAN_POINT ( 'NONE',  ( 10.39230484541326582, 0.000000000000000000, 5.000000000000000000 ) ) ;
#11167 = EDGE_CURVE ( 'NONE', #4465, #11247, #1507, .T. ) ;
#11169 = EDGE_CURVE ( 'NONE', #552, #6305, #228, .T. ) ;
#11168 = ADVANCED_FACE ( 'NONE', ( #11154 ), #1425, .F. ) ;
#11171 = AXIS2_PLACEMENT_3D ( 'NONE', #4966, #14501, #195 ) ;
#11170 = VECTOR ( 'NONE', #13422, 1000.000000000000000 ) ;
#11172 = DIRECTION ( 'NONE',  ( -1.000000000000000000, 0.000000000000000000, 0.000000000000000000 ) ) ;
#11173 = SURFACE_STYLE_USAGE ( .BOTH. , #7543 ) ;
#11174 = CARTESIAN_POINT ( 'NONE',  ( 205.3747499027128924, 33.81850075496041796, -3.363818451488727934 ) ) ;
#11175 = ORIENTED_EDGE ( 'NONE', *, *, #10203, .T. ) ;
#11176 = CARTESIAN_POINT ( 'NONE',  ( -110.0000000000000426, 59.53993994372674337, 25.00000000000000000 ) ) ;
#11177 = CARTESIAN_POINT ( 'NONE',  ( -223.3976496709624939, 142.4299982425674216, -0.2056757461415917587 ) ) ;
#11178 = CARTESIAN_POINT ( 'NONE',  ( -200.9686762702122849, 128.5620043109015853, -0.4555467707853345649 ) ) ;
#11179 = DIRECTION ( 'NONE',  ( 1.504267769033196424E-15, -0.9902680687415713612, -0.1391731009600591373 ) ) ;
#11180 = ORIENTED_EDGE ( 'NONE', *, *, #11550, .F. ) ;
#11181 = CARTESIAN_POINT ( 'NONE',  ( -175.7482920159357604, 118.3486081613139334, 7.749957389927518925 ) ) ;
#11182 = CIRCLE ( 'NONE', #4609, 1.699999999999998401 ) ;
#11183 = CARTESIAN_POINT ( 'NONE',  ( 198.8872864542346974, 32.16591232847088122, -2.310211674251309688 ) ) ;
#11184 = VERTEX_POINT ( 'NONE', #2460 ) ;
#11185 = ORIENTED_EDGE ( 'NONE', *, *, #8664, .F. ) ;
#11186 = STYLED_ITEM ( 'NONE', ( #514 ), #5622 ) ;
#11187 = DIRECTION ( 'NONE',  ( 0.000000000000000000, 0.000000000000000000, 1.000000000000000000 ) ) ;
#11188 = DIRECTION ( 'NONE',  ( 0.000000000000000000, 0.000000000000000000, 1.000000000000000000 ) ) ;
#11189 = DIRECTION ( 'NONE',  ( 0.000000000000000000, 1.000000000000000000, 6.938893903907227145E-17 ) ) ;
#11190 = CARTESIAN_POINT ( 'NONE',  ( -168.8345777152483151, 119.5835126658289909, 2.431557144026069928 ) ) ;
#11191 = CARTESIAN_POINT ( 'NONE',  ( -3.638415890883090848E-16, 2.111069397712021178, 1.843520544858951560 ) ) ;
#11192 = CARTESIAN_POINT ( 'NONE',  ( -206.8762397066792005, 149.3947262580036863, 3.478855109513426580 ) ) ;
#11193 = CARTESIAN_POINT ( 'NONE',  ( -85.99999999999994316, 62.13993994372673768, 15.00000000000174794 ) ) ;
#11194 = DIRECTION ( 'NONE',  ( -0.000000000000000000, 1.000000000000000000, 0.000000000000000000 ) ) ;
#11195 = ORIENTED_EDGE ( 'NONE', *, *, #4899, .F. ) ;
#11196 = FACE_BOUND ( 'NONE', #374, .T. ) ;
#11197 = EDGE_CURVE ( 'NONE', #15235, #4643, #8198, .T. ) ;
#11198 = ORIENTED_EDGE ( 'NONE', *, *, #7608, .T. ) ;
#11199 = EDGE_LOOP ( 'NONE', ( #5338, #10769, #3208, #11286 ) ) ;
#11200 = CARTESIAN_POINT ( 'NONE',  ( -86.77455057502459113, 65.19100426474074084, -20.00000000000000000 ) ) ;
#11201 = DIRECTION ( 'NONE',  ( 1.000000000000000000, 0.000000000000000000, 0.000000000000000000 ) ) ;
#11202 = AXIS2_PLACEMENT_3D ( 'NONE', #14898, #13882, #8926 ) ;
#11203 = FACE_BOUND ( 'NONE', #10315, .T. ) ;
#11204 = DIRECTION ( 'NONE',  ( 0.000000000000000000, 0.5000000000000006661, -0.8660254037844382635 ) ) ;
#11205 = B_SPLINE_CURVE_WITH_KNOTS ( 'NONE', 3,
 ( #3359, #7954, #8196, #12974, #1925, #5800, #6761, #15414, #9440, #2242, #7077, #6844, #11884, #735 ),
 .UNSPECIFIED., .F., .F.,
 ( 4, 2, 2, 2, 2, 2, 4 ),
 ( 0.003185368397584297136, 0.003588618066394599470, 0.003991867735204901804, 0.004798367072825479585, 0.005201616741635807506, 0.005604866410446135427, 0.006411365748066763515 ),
 .UNSPECIFIED. ) ;
#11206 = CARTESIAN_POINT ( 'NONE',  ( -219.7707515677084302, 153.4854131707639340, -0.3598758021188548373 ) ) ;
#11207 = CARTESIAN_POINT ( 'NONE',  ( -219.4661802592007689, 154.0311004795854046, 7.909502539118774322 ) ) ;
#11208 = AXIS2_PLACEMENT_3D ( 'NONE', #5454, #13647, #13892 ) ;
#11209 = ORIENTED_EDGE ( 'NONE', *, *, #1670, .T. ) ;
#11210 = CARTESIAN_POINT ( 'NONE',  ( 184.0000000000000568, -201.3058001507315566, -41.45141194869120227 ) ) ;
#11211 = CIRCLE ( 'NONE', #8454, 1.000000000000000888 ) ;
#11212 = CARTESIAN_POINT ( 'NONE',  ( 193.0950460371283839, 35.57958264137020876, -2.685405722344195389 ) ) ;
#11213 = ADVANCED_FACE ( 'NONE', ( #11228 ), #14452, .F. ) ;
#11214 = CARTESIAN_POINT ( 'NONE',  ( -223.8340338030139094, 146.2054052184961961, 6.383663356545733691 ) ) ;
#11215 = ORIENTED_EDGE ( 'NONE', *, *, #4283, .F. ) ;
#11216 = CARTESIAN_POINT ( 'NONE',  ( -221.1271579233365969, 151.0551982647748446, 7.614349089095027168 ) ) ;
#11217 = EDGE_LOOP ( 'NONE', ( #4031, #1937, #2451, #3224 ) ) ;
#11218 = CARTESIAN_POINT ( 'NONE',  ( -167.8641735700121558, 127.4776547538155853, 0.8902203665584077497 ) ) ;
#11219 = CARTESIAN_POINT ( 'NONE',  ( 190.0000000000000568, -178.8058001507315566, -30.31842631998718574 ) ) ;
#11220 = EDGE_LOOP ( 'NONE', ( #13128, #11861, #13627, #8020 ) ) ;
#11221 = DIRECTION ( 'NONE',  ( -1.000000000000000000, 0.000000000000000000, 3.965082230804112963E-16 ) ) ;
#11222 = CARTESIAN_POINT ( 'NONE',  ( -85.27455057502459113, 65.19100426474074084, 10.00000000000000178 ) ) ;
#11223 = AXIS2_PLACEMENT_3D ( 'NONE', #12278, #1458, #8984 ) ;
#11224 = DIRECTION ( 'NONE',  ( 0.000000000000000000, -0.000000000000000000, -1.000000000000000000 ) ) ;
#11225 = ORIENTED_EDGE ( 'NONE', *, *, #8173, .T. ) ;
#11226 = APPLICATION_PROTOCOL_DEFINITION ( 'draft international standard', 'automotive_design', 1998, #8388 ) ;
#11227 = VERTEX_POINT ( 'NONE', #4562 ) ;
#11228 = FACE_OUTER_BOUND ( 'NONE', #2760, .T. ) ;
#11229 = DIRECTION ( 'NONE',  ( -1.000000000000000000, 0.000000000000000000, 0.000000000000000000 ) ) ;
#11230 = EDGE_LOOP ( 'NONE', ( #11710, #6697, #14732, #12100 ) ) ;
#11231 = CARTESIAN_POINT ( 'NONE',  ( 73.76535645333923696, 38.79159067395544014, 10.00000000000000178 ) ) ;
#11232 = ADVANCED_FACE ( 'NONE', ( #3220 ), #10335, .F. ) ;
#11233 = CARTESIAN_POINT ( 'NONE',  ( 0.1090894304641069068, -2.915265454974089732, -0.4506121144344751306 ) ) ;
#11234 = ORIENTED_EDGE ( 'NONE', *, *, #6146, .T. ) ;
#11235 = VERTEX_POINT ( 'NONE', #5677 ) ;
#11236 = CARTESIAN_POINT ( 'NONE',  ( -85.27455057502459113, 65.19100426474074084, 10.00000000000000178 ) ) ;
#11237 = CARTESIAN_POINT ( 'NONE',  ( 191.4227524587821279, 39.61567282607229856, -2.929995994935606252 ) ) ;
#11238 = ORIENTED_EDGE ( 'NONE', *, *, #6243, .F. ) ;
#11239 = CARTESIAN_POINT ( 'NONE',  ( 201.8629198063431716, 32.54887535240757757, -8.146526315903498627 ) ) ;
#11240 = DIRECTION ( 'NONE',  ( 0.000000000000000000, 0.000000000000000000, 1.000000000000000000 ) ) ;
#11241 = DIRECTION ( 'NONE',  ( 0.000000000000000000, 0.000000000000000000, 1.000000000000000000 ) ) ;
#11242 = CARTESIAN_POINT ( 'NONE',  ( 190.0000000000000853, 14.90076684276667862, 37.08491613486884830 ) ) ;
#11243 = CARTESIAN_POINT ( 'NONE',  ( -63.50000000000002842, -179.8058001507315566, -51.45141194869120227 ) ) ;
#11244 = VECTOR ( 'NONE', #1823, 1000.000000000000114 ) ;
#11245 = EDGE_CURVE ( 'NONE', #457, #13965, #9387, .T. ) ;
#11246 = FILL_AREA_STYLE_COLOUR ( '', #8641 ) ;
#11247 = VERTEX_POINT ( 'NONE', #5223 ) ;
#11248 = CARTESIAN_POINT ( 'NONE',  ( 205.1062858801516597, 40.86394065090267702, -20.00000000000000000 ) ) ;
#11249 = CARTESIAN_POINT ( 'NONE',  ( -219.9272211304954681, 149.1032166049582486, -5.025525059679186057 ) ) ;
#11250 = CARTESIAN_POINT ( 'NONE',  ( -173.7777028115792177, 116.1670890754947152, -0.7095712321138001322 ) ) ;
#11252 = EDGE_CURVE ( 'NONE', #11722, #1879, #14106, .T. ) ;
#11251 = DIRECTION ( 'NONE',  ( 1.000000000000000000, 0.000000000000000000, 0.000000000000000000 ) ) ;
#11253 = ORIENTED_EDGE ( 'NONE', *, *, #1398, .T. ) ;
#11254 = CARTESIAN_POINT ( 'NONE',  ( -187.5349220100912930, 120.9938564418671518, 3.478895870929501921 ) ) ;
#11255 = CARTESIAN_POINT ( 'NONE',  ( 205.5140042898306660, 47.80506208259531320, -5.491262609045910459 ) ) ;
#11256 = EDGE_LOOP ( 'NONE', ( #8615, #1107, #3590, #15536 ) ) ;
#11257 = EDGE_CURVE ( 'NONE', #8794, #12311, #15473, .T. ) ;
#11258 = VECTOR ( 'NONE', #1985, 1000.000000000000000 ) ;
#11259 = AXIS2_PLACEMENT_3D ( 'NONE', #5435, #4876, #13145 ) ;
#11260 = CARTESIAN_POINT ( 'NONE',  ( -110.0000000000000426, 56.53993994372675047, 25.00000000000000000 ) ) ;
#11261 = DIRECTION ( 'NONE',  ( 1.000000000000000000, 0.000000000000000000, 0.000000000000000000 ) ) ;
#11262 = FACE_OUTER_BOUND ( 'NONE', #7568, .T. ) ;
#11263 = CARTESIAN_POINT ( 'NONE',  ( 184.0000000000000568, -201.3058001507315566, 74.95141194869098911 ) ) ;
#11264 = ORIENTED_EDGE ( 'NONE', *, *, #6842, .T. ) ;
#11265 = FACE_OUTER_BOUND ( 'NONE', #14696, .T. ) ;
#11266 = ADVANCED_FACE ( 'NONE', ( #4323 ), #7686, .F. ) ;
#11267 = EDGE_CURVE ( 'NONE', #1631, #8808, #6788, .T. ) ;
#11268 = CARTESIAN_POINT ( 'NONE',  ( -177.3600541072865155, 132.9204870282739819, 3.478855109513427468 ) ) ;
#11269 = FACE_OUTER_BOUND ( 'NONE', #9562, .T. ) ;
#11270 = DIRECTION ( 'NONE',  ( 0.000000000000000000, -1.000000000000000000, 0.000000000000000000 ) ) ;
#11271 = ORIENTED_EDGE ( 'NONE', *, *, #13957, .T. ) ;
#11272 = DIRECTION ( 'NONE',  ( 0.000000000000000000, -1.000000000000000000, -1.156482317317871478E-16 ) ) ;
#11273 = ORIENTED_EDGE ( 'NONE', *, *, #11318, .F. ) ;
#11274 = EDGE_LOOP ( 'NONE', ( #5731, #13844, #8041, #1709 ) ) ;
#11275 = CARTESIAN_POINT ( 'NONE',  ( -63.50000000000002842, -179.8058001507315566, 52.19066787724494816 ) ) ;
#11276 = CYLINDRICAL_SURFACE ( 'NONE', #4227, 0.5000000000000000000 ) ;
#11277 = CARTESIAN_POINT ( 'NONE',  ( 114.0000000000000568, 62.13993994372673768, 11.50000000000034817 ) ) ;
#11278 = CARTESIAN_POINT ( 'NONE',  ( -217.5316743144719567, 153.4425273680139696, -2.341497464274004070 ) ) ;
#11279 = ORIENTED_EDGE ( 'NONE', *, *, #9029, .T. ) ;
#11280 = ADVANCED_FACE ( 'NONE', ( #4404 ), #6683, .T. ) ;
#11281 = CARTESIAN_POINT ( 'NONE',  ( -76.00000000000001421, -179.3058001507315566, -30.31842631998718574 ) ) ;
#11282 = CARTESIAN_POINT ( 'NONE',  ( 205.4319281802536068, 33.87189768065903905, -1.932853472788024440 ) ) ;
#11283 = CARTESIAN_POINT ( 'NONE',  ( -221.0392844523545364, 151.2126373818472871, -2.672071522959135415 ) ) ;
#11284 = ORIENTED_EDGE ( 'NONE', *, *, #2047, .T. ) ;
#11285 = CARTESIAN_POINT ( 'NONE',  ( -220.1509919453162638, 152.8041528465324461, 8.810372448773614806 ) ) ;
#11286 = ORIENTED_EDGE ( 'NONE', *, *, #14626, .F. ) ;
#11287 = CARTESIAN_POINT ( 'NONE',  ( -169.5742008144607098, 124.4138725163886505, -4.326550720942743844 ) ) ;
#11288 = PLANE ( 'NONE',  #7366 ) ;
#11289 = ORIENTED_EDGE ( 'NONE', *, *, #14306, .F. ) ;
#11290 = LINE ( 'NONE', #4102, #11715 ) ;
#11291 = CARTESIAN_POINT ( 'NONE',  ( 5.799999999999999822, -6.928203230275514990, -4.000000000000003553 ) ) ;
#11292 = AXIS2_PLACEMENT_3D ( 'NONE', #13237, #8228, #1240 ) ;
#11293 = EDGE_CURVE ( 'NONE', #13094, #256, #4032, .T. ) ;
#11294 = FACE_OUTER_BOUND ( 'NONE', #3164, .T. ) ;
#11295 = ORIENTED_EDGE ( 'NONE', *, *, #8976, .F. ) ;
#11296 = VECTOR ( 'NONE', #2350, 1000.000000000000000 ) ;
#11297 = DIRECTION ( 'NONE',  ( 0.8490470260013033288, -0.5283172793297058467, 0.000000000000000000 ) ) ;
#11298 = ORIENTED_EDGE ( 'NONE', *, *, #11447, .F. ) ;
#11299 = CARTESIAN_POINT ( 'NONE',  ( 166.3583383998781358, 57.46267437295986014, 0.000000000000000000 ) ) ;
#11300 = PLANE ( 'NONE',  #6513 ) ;
#11301 = ORIENTED_EDGE ( 'NONE', *, *, #14726, .T. ) ;
#11302 = DIRECTION ( 'NONE',  ( 0.000000000000000000, -5.551115123125777653E-14, -1.000000000000000000 ) ) ;
#11303 = VECTOR ( 'NONE', #12482, 1000.000000000000000 ) ;
#11304 = DIRECTION ( 'NONE',  ( 0.6130913241491353638, 0.7900120431063440973, -6.390853288715849130E-17 ) ) ;
#11305 = VERTEX_POINT ( 'NONE', #922 ) ;
#11306 = ORIENTED_EDGE ( 'NONE', *, *, #1445, .F. ) ;
#11307 = CARTESIAN_POINT ( 'NONE',  ( -76.50000000000004263, 14.90076684276667507, 37.08491613486882699 ) ) ;
#11308 = CARTESIAN_POINT ( 'NONE',  ( 207.1164837741930569, 35.57719129110033407, -1.806778302941847159 ) ) ;
#11309 = CIRCLE ( 'NONE', #8547, 0.5000000000000069944 ) ;
#11310 = ORIENTED_EDGE ( 'NONE', *, *, #12226, .T. ) ;
#11312 = EDGE_CURVE ( 'NONE', #6346, #12639, #5748, .T. ) ;
#11311 = CARTESIAN_POINT ( 'NONE',  ( 198.8634854004546071, 49.55149448133588663, -6.680369717582868461 ) ) ;
#11313 = CARTESIAN_POINT ( 'NONE',  ( -223.6145774380523505, 142.0129443944823606, 2.393984899497048513 ) ) ;
#11314 = CYLINDRICAL_SURFACE ( 'NONE', #4007, 338.5619230110239641 ) ;
#11315 = LINE ( 'NONE', #5400, #14765 ) ;
#11316 = CARTESIAN_POINT ( 'NONE',  ( -64.00000000000002842, 15.03993994372673981, 10.05257423913146475 ) ) ;
#11317 = VECTOR ( 'NONE', #9798, 1000.000000000000000 ) ;
#11318 = EDGE_CURVE ( 'NONE', #12158, #944, #11211, .T. ) ;
#11319 = TOROIDAL_SURFACE ( 'NONE', #11822, 1.000000000000000000, 0.5000000000000000000 ) ;
#11320 = CARTESIAN_POINT ( 'NONE',  ( -156.6477983077465410, 110.1970436846185066, 5.000000000000000000 ) ) ;
#11321 = ORIENTED_EDGE ( 'NONE', *, *, #9725, .T. ) ;
#11322 = EDGE_CURVE ( 'NONE', #8914, #3938, #6432, .T. ) ;
#11323 = FACE_OUTER_BOUND ( 'NONE', #7211, .T. ) ;
#11324 = CARTESIAN_POINT ( 'NONE',  ( -191.1563096742665380, 133.0698578461479826, -5.230826428279597984 ) ) ;
#11325 = DIRECTION ( 'NONE',  ( 0.000000000000000000, -1.156482317317871725E-16, 1.000000000000000000 ) ) ;
#11326 = ORIENTED_EDGE ( 'NONE', *, *, #2880, .F. ) ;
#11327 = CARTESIAN_POINT ( 'NONE',  ( -179.3772030532177837, 117.5545944912402661, 1.382365641875445528 ) ) ;
#11328 = CARTESIAN_POINT ( 'NONE',  ( 205.4727397017886119, 47.82775141623291404, -2.488642475836487566 ) ) ;
#11329 = ORIENTED_EDGE ( 'NONE', *, *, #13348, .F. ) ;
#11330 = AXIS2_PLACEMENT_3D ( 'NONE', #6191, #3578, #14614 ) ;
#11331 = DIRECTION ( 'NONE',  ( -1.000000000000000000, 0.000000000000000000, 0.000000000000000000 ) ) ;
#11332 = CARTESIAN_POINT ( 'NONE',  ( -64.00000000000002842, 15.03993994372673981, 10.05257423913146475 ) ) ;
#11333 = CARTESIAN_POINT ( 'NONE',  ( 170.6931741512129577, -3.595212766542494887, -13.46247879130521952 ) ) ;
#11334 = EDGE_CURVE ( 'NONE', #5911, #10463, #9698, .T. ) ;
#11335 = AXIS2_PLACEMENT_3D ( 'NONE', #4787, #9612, #5817 ) ;
#11336 = VECTOR ( 'NONE', #5484, 999.9999999999998863 ) ;
#11337 = CIRCLE ( 'NONE', #8339, 1.699999999999993072 ) ;
#11338 = LINE ( 'NONE', #3052, #14157 ) ;
#11339 = EDGE_LOOP ( 'NONE', ( #11532, #14958, #1636, #7151 ) ) ;
#11340 = CIRCLE ( 'NONE', #4530, 2.749999999999999112 ) ;
#11341 = DIRECTION ( 'NONE',  ( -0.000000000000000000, -0.000000000000000000, 1.000000000000000000 ) ) ;
#11342 = CARTESIAN_POINT ( 'NONE',  ( 215.1062858801516882, 25.86394065090268057, 18.00000000000000355 ) ) ;
#11343 = DIRECTION ( 'NONE',  ( 1.000000000000000000, 0.000000000000000000, 0.000000000000000000 ) ) ;
#11344 = VERTEX_POINT ( 'NONE', #6870 ) ;
#11345 = CARTESIAN_POINT ( 'NONE',  ( 190.0000000000000568, 15.53993994372673804, 24.94742576086838781 ) ) ;
#11346 = ORIENTED_EDGE ( 'NONE', *, *, #1567, .T. ) ;
#11347 = ORIENTED_EDGE ( 'NONE', *, *, #13850, .T. ) ;
#11348 = DIRECTION ( 'NONE',  ( 5.518327896226364679E-17, 0.9902680687415713612, -0.1391731009600582492 ) ) ;
#11349 = DIRECTION ( 'NONE',  ( -0.000000000000000000, 1.000000000000000000, 0.000000000000000000 ) ) ;
#11350 = CONICAL_SURFACE ( 'NONE', #2276, 8.000000000000028422, 1.047197551196600296 ) ;
#11351 = DIRECTION ( 'NONE',  ( -0.000000000000000000, -0.000000000000000000, 1.000000000000000000 ) ) ;
#11352 = CONICAL_SURFACE ( 'NONE', #13359, 3.525000000000000355, 0.7853981633973787790 ) ;
#11353 = CARTESIAN_POINT ( 'NONE',  ( -35.99999999999995026, 59.53993994372674337, 16.70000000000140261 ) ) ;
#11354 = DIRECTION ( 'NONE',  ( 0.000000000000000000, 0.000000000000000000, -1.000000000000000000 ) ) ;
#11355 = CARTESIAN_POINT ( 'NONE',  ( -219.5587625787842114, 153.8652247210798123, 0.6104961448661524459 ) ) ;
#11356 = EDGE_CURVE ( 'NONE', #14280, #15168, #2887, .T. ) ;
#11357 = EDGE_CURVE ( 'NONE', #11465, #8395, #8866, .T. ) ;
#11358 = ADVANCED_FACE ( 'NONE', ( #677 ), #7432, .T. ) ;
#11359 = DIRECTION ( 'NONE',  ( -1.000000000000000000, 0.000000000000000000, 0.000000000000000000 ) ) ;
#11360 = VERTEX_POINT ( 'NONE', #11598 ) ;
#11361 = FACE_OUTER_BOUND ( 'NONE', #11220, .T. ) ;
#11362 = UNCERTAINTY_MEASURE_WITH_UNIT (LENGTH_MEASURE( 1.000000000000000082E-05 ), #1061, 'distance_accuracy_value', 'NONE');
#11363 = AXIS2_PLACEMENT_3D ( 'NONE', #452, #4103, #6415 ) ;
#11364 = PLANE ( 'NONE',  #11698 ) ;
#11365 = CIRCLE ( 'NONE', #2794, 1.700000000000007061 ) ;
#11366 = CIRCLE ( 'NONE', #10106, 3.525000000000000355 ) ;
#11367 = CARTESIAN_POINT ( 'NONE',  ( 201.2658342953964166, 49.58143373454755931, -3.806719548689701416 ) ) ;
#11368 = DIRECTION ( 'NONE',  ( 0.000000000000000000, 0.000000000000000000, 1.000000000000000000 ) ) ;
#11369 = ORIENTED_EDGE ( 'NONE', *, *, #8346, .F. ) ;
#11370 = CARTESIAN_POINT ( 'NONE',  ( -216.9389196770082151, 154.4740194435295564, 5.145036412574403251 ) ) ;
#11371 = ORIENTED_EDGE ( 'NONE', *, *, #9692, .F. ) ;
#11372 = CARTESIAN_POINT ( 'NONE',  ( -172.3934359946532311, 119.3627701458021875, -4.525325099609154300 ) ) ;
#11373 = PLANE ( 'NONE',  #8870 ) ;
#11374 = VERTEX_POINT ( 'NONE', #3146 ) ;
#11375 = DIRECTION ( 'NONE',  ( 0.000000000000000000, 0.000000000000000000, -1.000000000000000000 ) ) ;
#11376 = DIRECTION ( 'NONE',  ( 1.000000000000000000, 0.000000000000000000, 0.000000000000000000 ) ) ;
#11377 = AXIS2_PLACEMENT_3D ( 'NONE', #6386, #11194, #13308 ) ;
#11378 = VECTOR ( 'NONE', #3734, 1000.000000000000000 ) ;
#11379 = DIRECTION ( 'NONE',  ( 0.000000000000000000, 0.000000000000000000, 1.000000000000000000 ) ) ;
#11380 = EDGE_LOOP ( 'NONE', ( #3572, #9942, #4349, #6829 ) ) ;
#11381 = ITEM_DEFINED_TRANSFORMATION ( 'NONE', 'NONE', #15077,  #12337 ) ;
#11382 = EDGE_LOOP ( 'NONE', ( #9244, #3001, #7555, #314, #14768, #13737 ) ) ;
#11383 = DIRECTION ( 'NONE',  ( 2.751328491981765035E-32, 1.000000000000000000, 1.090924371466202084E-47 ) ) ;
#11384 = ORIENTED_EDGE ( 'NONE', *, *, #4596, .F. ) ;
#11385 = CYLINDRICAL_SURFACE ( 'NONE', #2415, 59.90987050789675550 ) ;
#11386 = CIRCLE ( 'NONE', #13389, 8.000000000000028422 ) ;
#11387 = DIRECTION ( 'NONE',  ( 0.000000000000000000, 0.000000000000000000, 1.000000000000000000 ) ) ;
#11388 = ORIENTED_EDGE ( 'NONE', *, *, #10607, .F. ) ;
#11389 = ORIENTED_EDGE ( 'NONE', *, *, #4214, .T. ) ;
#11390 = CARTESIAN_POINT ( 'NONE',  ( -177.3557003870508595, 132.9282874014947140, 2.500000000000000000 ) ) ;
#11391 = DIRECTION ( 'NONE',  ( 1.000000000000000000, 0.000000000000000000, 0.000000000000000000 ) ) ;
#11392 = EDGE_CURVE ( 'NONE', #5020, #14786, #12765, .T. ) ;
#11393 = ORIENTED_EDGE ( 'NONE', *, *, #4754, .F. ) ;
#11394 = CARTESIAN_POINT ( 'NONE',  ( 194.8381067511959372, 47.88228248201940573, -3.436395123936771601 ) ) ;
#11395 = CARTESIAN_POINT ( 'NONE',  ( -135.3034657297974093, 107.4444500778096483, 5.000000000000000000 ) ) ;
#11396 = LINE ( 'NONE', #11165, #7831 ) ;
#11397 = CARTESIAN_POINT ( 'NONE',  ( -70.00000000000000000, 15.53993994372673626, 45.99999999999998579 ) ) ;
#11398 = DIRECTION ( 'NONE',  ( 0.000000000000000000, 0.000000000000000000, -1.000000000000000000 ) ) ;
#11399 = VECTOR ( 'NONE', #13238, 1000.000000000000000 ) ;
#11400 = VECTOR ( 'NONE', #14186, 1000.000000000000227 ) ;
#11401 = DIRECTION ( 'NONE',  ( 0.000000000000000000, -1.000000000000000000, 0.000000000000000000 ) ) ;
#11402 = ORIENTED_EDGE ( 'NONE', *, *, #11245, .F. ) ;
#11403 = DIRECTION ( 'NONE',  ( -0.000000000000000000, -0.000000000000000000, 1.000000000000000000 ) ) ;
#11404 = CARTESIAN_POINT ( 'NONE',  ( -173.2995934586704152, 128.4510609142004114, -2.983067475588502937 ) ) ;
#11405 = DIRECTION ( 'NONE',  ( 0.7071067811865474617, 0.000000000000000000, 0.7071067811865474617 ) ) ;
#11406 = ORIENTED_EDGE ( 'NONE', *, *, #7991, .T. ) ;
#11407 = EDGE_CURVE ( 'NONE', #13191, #10895, #9957, .T. ) ;
#11408 = CARTESIAN_POINT ( 'NONE',  ( -191.4964613557999655, 125.7493975051623352, 3.478895870929489043 ) ) ;
#11410 = CARTESIAN_POINT ( 'NONE',  ( 190.5897039592268243, 47.97531786402677056, -7.885730391161881236 ) ) ;
#11409 = CIRCLE ( 'NONE', #1816, 325.5619230110239073 ) ;
#11411 = ORIENTED_EDGE ( 'NONE', *, *, #12547, .T. ) ;
#11412 = AXIS2_PLACEMENT_3D ( 'NONE', #3697, #14578, #8526 ) ;
#11413 = LINE ( 'NONE', #7637, #6678 ) ;
#11414 = CARTESIAN_POINT ( 'NONE',  ( 0.000000000000000000, -7.511572993685817836E-16, 2.749999999999999112 ) ) ;
#11415 = ADVANCED_FACE ( 'NONE', ( #4881 ), #9623, .T. ) ;
#11416 = FACE_OUTER_BOUND ( 'NONE', #14085, .T. ) ;
#11417 = CARTESIAN_POINT ( 'NONE',  ( 120.8806775638430224, 45.00321902537314145, 10.00000000000000178 ) ) ;
#11418 = ORIENTED_EDGE ( 'NONE', *, *, #3187, .T. ) ;
#11419 = DIRECTION ( 'NONE',  ( -0.4460111024107797362, -0.8950274278067241740, 0.000000000000000000 ) ) ;
#11420 = CARTESIAN_POINT ( 'NONE',  ( -183.7478807014743722, 127.6480629723144347, 10.16010209732750624 ) ) ;
#11421 = CARTESIAN_POINT ( 'NONE',  ( 14.00000000000004086, 64.53993994372673626, 15.00000000000104983 ) ) ;
#11422 = CARTESIAN_POINT ( 'NONE',  ( 120.8806775638430224, 45.00321902537314145, 0.000000000000000000 ) ) ;
#11423 = PRODUCT_DEFINITION_SHAPE ( 'NONE', 'NONE',  #15630 ) ;
#11424 = ORIENTED_EDGE ( 'NONE', *, *, #5368, .T. ) ;
#11425 = AXIS2_PLACEMENT_3D ( 'NONE', #9871, #8684, #7351 ) ;
#11426 = CARTESIAN_POINT ( 'NONE',  ( 114.0000000000000568, 62.13993994372673768, 16.70000000000034746 ) ) ;
#11427 = ADVANCED_FACE ( 'NONE', ( #5984 ), #14416, .F. ) ;
#11428 = ORIENTED_EDGE ( 'NONE', *, *, #5465, .T. ) ;
#11429 = ORIENTED_EDGE ( 'NONE', *, *, #8860, .F. ) ;
#11430 = CARTESIAN_POINT ( 'NONE',  ( -150.4086188282879277, 107.2728346664360259, 9.719846845941791713 ) ) ;
#11431 = DIRECTION ( 'NONE',  ( -0.000000000000000000, -0.000000000000000000, -1.000000000000000000 ) ) ;
#11432 = CARTESIAN_POINT ( 'NONE',  ( -155.6477983077465410, 110.1970436846185066, -4.856732557889651858 ) ) ;
#11433 = CARTESIAN_POINT ( 'NONE',  ( 0.000000000000000000, 0.000000000000000000, 0.000000000000000000 ) ) ;
#11434 = CIRCLE ( 'NONE', #10936, 1.499999999999992228 ) ;
#11435 = ADVANCED_FACE ( 'NONE', ( #1232 ), #6170, .T. ) ;
#11436 = CARTESIAN_POINT ( 'NONE',  ( 224.0000000000000853, 56.53993994372675047, 25.00000000000000000 ) ) ;
#11437 = AXIS2_PLACEMENT_3D ( 'NONE', #4086, #1867, #12606 ) ;
#11438 = CARTESIAN_POINT ( 'NONE',  ( -156.6477983077465410, 110.1970436846185066, 0.000000000000000000 ) ) ;
#11439 = CARTESIAN_POINT ( 'NONE',  ( -76.50000000000001421, 17.53993994372674692, -17.50000000000002487 ) ) ;
#11440 = EDGE_CURVE ( 'NONE', #10266, #4760, #12957, .T. ) ;
#11441 = DIRECTION ( 'NONE',  ( 0.000000000000000000, 0.000000000000000000, -1.000000000000000000 ) ) ;
#11442 = CARTESIAN_POINT ( 'NONE',  ( -221.3648744334925027, 150.6292918216330179, -2.896295222704587946 ) ) ;
#11443 = ORIENTED_EDGE ( 'NONE', *, *, #2882, .T. ) ;
#11444 = CIRCLE ( 'NONE', #4123, 0.5000000000000004441 ) ;
#11445 = CARTESIAN_POINT ( 'NONE',  ( -220.2190305748135586, 148.6074564430024054, 9.948829861901575811 ) ) ;
#11447 = EDGE_CURVE ( 'NONE', #5262, #9103, #7926, .T. ) ;
#11446 = ADVANCED_FACE ( 'NONE', ( #6147 ), #999, .F. ) ;
#11448 = ORIENTED_EDGE ( 'NONE', *, *, #13694, .F. ) ;
#11449 = EDGE_CURVE ( 'NONE', #6079, #3829, #11830, .T. ) ;
#11450 = CARTESIAN_POINT ( 'NONE',  ( 0.01688885742777454860, -7.321065037175440438, -3.319543390096036273 ) ) ;
#11451 = DIRECTION ( 'NONE',  ( -1.000000000000000000, 0.000000000000000000, 0.000000000000000000 ) ) ;
#11453 = ORIENTED_EDGE ( 'NONE', *, *, #15575, .T. ) ;
#11452 = AXIS2_PLACEMENT_3D ( 'NONE', #4212, #2816, #4064 ) ;
#11454 = DIRECTION ( 'NONE',  ( 1.000000000000000000, -2.751328491981765035E-32, 3.965082230804130220E-16 ) ) ;
#11455 = CARTESIAN_POINT ( 'NONE',  ( 200.1062858801516597, 40.86394065090267702, 0.000000000000000000 ) ) ;
#11456 = EDGE_CURVE ( 'NONE', #10340, #7288, #5906, .T. ) ;
#11457 = DIRECTION ( 'NONE',  ( 1.000000000000000000, 0.000000000000000000, 0.000000000000000000 ) ) ;
#11458 = ORIENTED_EDGE ( 'NONE', *, *, #9927, .F. ) ;
#11459 = PRESENTATION_LAYER_ASSIGNMENT (  '', '', ( #14469 ) ) ;
#11460 = SHAPE_DEFINITION_REPRESENTATION ( #11552, #7041 ) ;
#11461 = EDGE_LOOP ( 'NONE', ( #1536, #9328, #11175, #3911, #4656, #6879 ) ) ;
#11462 = CIRCLE ( 'NONE', #62, 3.525000000000000355 ) ;
#11463 = CARTESIAN_POINT ( 'NONE',  ( 201.1780093772972009, 32.12620995903681376, -3.617034841014101776 ) ) ;
#11464 = DIRECTION ( 'NONE',  ( -0.000000000000000000, 0.000000000000000000, 1.000000000000000000 ) ) ;
#11465 = VERTEX_POINT ( 'NONE', #114 ) ;
#11466 = LINE ( 'NONE', #14921, #11244 ) ;
#11467 = ADVANCED_FACE ( 'NONE', ( #13305 ), #4956, .T. ) ;
#11468 = EDGE_CURVE ( 'NONE', #5691, #14996, #7943, .T. ) ;
#11469 = CARTESIAN_POINT ( 'NONE',  ( -136.1405586187959784, 108.3975249866138597, 0.000000000000000000 ) ) ;
#11470 = ORIENTED_EDGE ( 'NONE', *, *, #747, .F. ) ;
#11471 = ORIENTED_EDGE ( 'NONE', *, *, #2664, .F. ) ;
#11472 = DIRECTION ( 'NONE',  ( 0.000000000000000000, 0.1391731009600626345, 0.9902680687415706950 ) ) ;
#11473 = FACE_OUTER_BOUND ( 'NONE', #3742, .T. ) ;
#11474 = AXIS2_PLACEMENT_3D ( 'NONE', #11662, #10544, #2096 ) ;
#11475 = ORIENTED_EDGE ( 'NONE', *, *, #362, .F. ) ;
#11476 = DIRECTION ( 'NONE',  ( 1.000000000000000000, 0.000000000000000000, 0.000000000000000000 ) ) ;
#11477 = LINE ( 'NONE', #14850, #13872 ) ;
#11478 = EDGE_CURVE ( 'NONE', #12734, #9960, #10648, .T. ) ;
#11479 = FACE_OUTER_BOUND ( 'NONE', #7890, .T. ) ;
#11480 = DIRECTION ( 'NONE',  ( 0.000000000000000000, 0.000000000000000000, 1.000000000000000000 ) ) ;
#11481 = CARTESIAN_POINT ( 'NONE',  ( -64.00000000000002842, -179.3058001507315566, 84.88378295107887084 ) ) ;
#11482 = ADVANCED_FACE ( 'NONE', ( #9464 ), #14263, .T. ) ;
#11483 = CIRCLE ( 'NONE', #9220, 1.000000000000000888 ) ;
#11484 = DIRECTION ( 'NONE',  ( 0.000000000000000000, 0.000000000000000000, -1.000000000000000000 ) ) ;
#11485 = ORIENTED_EDGE ( 'NONE', *, *, #15322, .T. ) ;
#11486 = DIRECTION ( 'NONE',  ( -0.000000000000000000, 1.000000000000000000, -0.000000000000000000 ) ) ;
#11487 = CARTESIAN_POINT ( 'NONE',  ( -194.7245433579248868, 140.1837011942588447, -2.963320117457102665 ) ) ;
#11488 = CARTESIAN_POINT ( 'NONE',  ( -85.99999999999994316, 62.13993994372673768, 11.50000000000174438 ) ) ;
#11489 = ORIENTED_EDGE ( 'NONE', *, *, #1625, .T. ) ;
#11490 = CARTESIAN_POINT ( 'NONE',  ( -217.9771163551940276, 139.5700662992579737, 5.434137442415948982 ) ) ;
#11491 = CARTESIAN_POINT ( 'NONE',  ( 190.6178699541428898, 33.66405957396897719, -4.118459193090428627 ) ) ;
#11492 = ORIENTED_EDGE ( 'NONE', *, *, #6610, .T. ) ;
#11493 = AXIS2_PLACEMENT_3D ( 'NONE', #9023, #13740, #7763 ) ;
#11494 = CARTESIAN_POINT ( 'NONE',  ( -63.50000000000002842, 15.03993994372673804, 24.94742576086838781 ) ) ;
#11495 = DIRECTION ( 'NONE',  ( 0.000000000000000000, 0.000000000000000000, 1.000000000000000000 ) ) ;
#11496 = VECTOR ( 'NONE', #10938, 1000.000000000000000 ) ;
#11497 = DIRECTION ( 'NONE',  ( -0.000000000000000000, 1.000000000000000000, -0.000000000000000000 ) ) ;
#11498 = DIRECTION ( 'NONE',  ( 1.000000000000000000, 0.000000000000000000, 0.000000000000000000 ) ) ;
#11499 = EDGE_CURVE ( 'NONE', #14095, #13329, #14877, .T. ) ;
#11500 = LINE ( 'NONE', #11417, #8525 ) ;
#11501 = ORIENTED_EDGE ( 'NONE', *, *, #8939, .T. ) ;
#11502 = CARTESIAN_POINT ( 'NONE',  ( 64.00000000000005684, 64.53993994372673626, 15.00000000000070166 ) ) ;
#11503 = CIRCLE ( 'NONE', #8985, 0.5000000000000004441 ) ;
#11504 = CARTESIAN_POINT ( 'NONE',  ( -189.9062345257129323, 135.2872556402745374, 9.578254705571842109 ) ) ;
#11505 = CYLINDRICAL_SURFACE ( 'NONE', #7535, 0.5000000000000004441 ) ;
#11506 = CARTESIAN_POINT ( 'NONE',  ( 177.5000000000000853, -181.3058001507315566, 84.88378295107885663 ) ) ;
#11507 = ORIENTED_EDGE ( 'NONE', *, *, #10235, .T. ) ;
#11508 = CONICAL_SURFACE ( 'NONE', #8496, 3.525000000000000355, 0.7853981633974482790 ) ;
#11509 = DIRECTION ( 'NONE',  ( -0.000000000000000000, 1.000000000000000000, -0.000000000000000000 ) ) ;
#11510 = VERTEX_POINT ( 'NONE', #13535 ) ;
#11511 = VERTEX_POINT ( 'NONE', #10162 ) ;
#11512 = CARTESIAN_POINT ( 'NONE',  ( -152.2906842424466163, 107.7605580766055766, 9.583914075210632433 ) ) ;
#11513 = CARTESIAN_POINT ( 'NONE',  ( 5.799999999999999822, -4.618802153516981868, 8.000000000000007105 ) ) ;
#11514 = CARTESIAN_POINT ( 'NONE',  ( -174.0411197980623399, 116.4106859692672629, 5.128256677369954275 ) ) ;
#11515 = CARTESIAN_POINT ( 'NONE',  ( -220.8828325425079981, 151.4929455371446920, -2.526440128526473039 ) ) ;
#11516 = DIRECTION ( 'NONE',  ( 0.000000000000000000, 8.673617379884035472E-17, -1.000000000000000000 ) ) ;
#11517 = CIRCLE ( 'NONE', #13516, 3.500000000000001332 ) ;
#11518 = DIRECTION ( 'NONE',  ( 3.965082230804130220E-16, -4.956352788505162775E-17, 1.000000000000000000 ) ) ;
#11519 = FACE_OUTER_BOUND ( 'NONE', #1064, .T. ) ;
#11520 = ADVANCED_FACE ( 'NONE', ( #6297 ), #4072, .F. ) ;
#11521 = FACE_BOUND ( 'NONE', #13019, .T. ) ;
#11522 = CARTESIAN_POINT ( 'NONE',  ( -220.5827524466467082, 152.0305861335090185, -2.167411312480779007 ) ) ;
#11523 = EDGE_LOOP ( 'NONE', ( #10954, #15544, #1553, #5449 ) ) ;
#11524 = ORIENTED_EDGE ( 'NONE', *, *, #11734, .T. ) ;
#11525 = DIRECTION ( 'NONE',  ( 0.000000000000000000, 0.000000000000000000, -1.000000000000000000 ) ) ;
#11526 = CARTESIAN_POINT ( 'NONE',  ( 6.399999999999999467, 0.000000000000000000, 0.000000000000000000 ) ) ;
#11527 = CARTESIAN_POINT ( 'NONE',  ( -76.50000000000001421, 16.03993994372673981, -17.50000000000002487 ) ) ;
#11528 = DIRECTION ( 'NONE',  ( -0.000000000000000000, 1.000000000000000000, -0.000000000000000000 ) ) ;
#11529 = DIRECTION ( 'NONE',  ( -0.000000000000000000, 1.000000000000000000, -0.000000000000000000 ) ) ;
#11530 = EDGE_CURVE ( 'NONE', #9186, #1354, #6609, .T. ) ;
#11531 = PLANE ( 'NONE',  #12416 ) ;
#11532 = ORIENTED_EDGE ( 'NONE', *, *, #3139, .F. ) ;
#11533 = EDGE_CURVE ( 'NONE', #4096, #5874, #13472, .T. ) ;
#11534 = ORIENTED_EDGE ( 'NONE', *, *, #1087, .F. ) ;
#11535 = CARTESIAN_POINT ( 'NONE',  ( 190.5897039592268243, 47.97531786402677056, -7.885730391161881236 ) ) ;
#11536 = ADVANCED_FACE ( 'NONE', ( #11265 ), #420, .T. ) ;
#11537 = VERTEX_POINT ( 'NONE', #345 ) ;
#11538 = DIRECTION ( 'NONE',  ( 0.4873681696970831312, 0.8731965799097676229, 0.000000000000000000 ) ) ;
#11539 = ORIENTED_EDGE ( 'NONE', *, *, #12964, .F. ) ;
#11540 = ORIENTED_EDGE ( 'NONE', *, *, #12087, .F. ) ;
#11541 = DIRECTION ( 'NONE',  ( -1.000000000000000000, 0.000000000000000000, 0.000000000000000000 ) ) ;
#11542 = CARTESIAN_POINT ( 'NONE',  ( -105.7032403413611661, 68.63699971342407480, 5.000000000000000000 ) ) ;
#11543 = VERTEX_POINT ( 'NONE', #3987 ) ;
#11544 = CARTESIAN_POINT ( 'NONE',  ( 207.1194509196011495, 46.14302886020001182, -1.185720282267065828 ) ) ;
#11545 = CARTESIAN_POINT ( 'NONE',  ( -168.8345777152483151, 119.5835126658289909, 2.431557144026069928 ) ) ;
#11546 = CARTESIAN_POINT ( 'NONE',  ( -76.50000000000004263, 17.53993994372673271, 52.49999999999997868 ) ) ;
#11547 = DIRECTION ( 'NONE',  ( -1.000000000000000000, 0.000000000000000000, -0.000000000000000000 ) ) ;
#11548 = CYLINDRICAL_SURFACE ( 'NONE', #12351, 1.699999999999991518 ) ;
#11549 = ADVANCED_FACE ( 'NONE', ( #9933 ), #1628, .F. ) ;
#11550 = EDGE_CURVE ( 'NONE', #868, #2171, #6693, .T. ) ;
#11551 = ADVANCED_FACE ( 'NONE', ( #13778 ), #14954, .T. ) ;
#11552 = PRODUCT_DEFINITION_SHAPE ( 'NONE', 'NONE',  #10574 ) ;
#11553 = AXIS2_PLACEMENT_3D ( 'NONE', #7054, #5931, #3567 ) ;
#11554 = CARTESIAN_POINT ( 'NONE',  ( 0.000000000000000000, 0.000000000000000000, 0.000000000000000000 ) ) ;
#11555 =( GEOMETRIC_REPRESENTATION_CONTEXT ( 3 ) GLOBAL_UNCERTAINTY_ASSIGNED_CONTEXT ( ( #3426 ) ) GLOBAL_UNIT_ASSIGNED_CONTEXT ( ( #15053, #8062, #4327 ) ) REPRESENTATION_CONTEXT ( 'NONE', 'WORKASPACE' ) );
#11556 = ORIENTED_EDGE ( 'NONE', *, *, #10311, .T. ) ;
#11557 = LINE ( 'NONE', #721, #1887 ) ;
#11558 = AXIS2_PLACEMENT_3D ( 'NONE', #1857, #14013, #6700 ) ;
#11559 = CARTESIAN_POINT ( 'NONE',  ( -180.9555975561403613, 132.5588568579215973, -2.963320117457099112 ) ) ;
#11560 = CARTESIAN_POINT ( 'NONE',  ( -5.000000000000000000, 0.000000000000000000, 5.000000000000000000 ) ) ;
#11561 = ORIENTED_EDGE ( 'NONE', *, *, #4940, .T. ) ;
#11562 = CARTESIAN_POINT ( 'NONE',  ( -197.4248861630254055, 135.1594620591177431, -5.230826428279599760 ) ) ;
#11563 = CARTESIAN_POINT ( 'NONE',  ( 201.8058794277662571, 52.63602710067958412, -5.247041060177010330 ) ) ;
#11564 = ORIENTED_EDGE ( 'NONE', *, *, #10607, .T. ) ;
#11565 = EDGE_CURVE ( 'NONE', #11151, #259, #6539, .T. ) ;
#11566 = CIRCLE ( 'NONE', #4750, 3.500000000000003109 ) ;
#11567 = DIRECTION ( 'NONE',  ( -3.965082230804130220E-16, 4.956352788505162775E-17, -1.000000000000000000 ) ) ;
#11568 = LINE ( 'NONE', #10156, #4673 ) ;
#11569 = CARTESIAN_POINT ( 'NONE',  ( -63.50000000000002842, -179.3058001507315566, -51.45141194869120227 ) ) ;
#11570 = CIRCLE ( 'NONE', #1481, 0.5000000000000004441 ) ;
#11571 = AXIS2_PLACEMENT_3D ( 'NONE', #12827, #902, #3289 ) ;
#11572 = DIRECTION ( 'NONE',  ( 0.4873681696970831312, 0.8731965799097676229, 0.000000000000000000 ) ) ;
#11573 = ORIENTED_EDGE ( 'NONE', *, *, #8852, .F. ) ;
#11574 = DIRECTION ( 'NONE',  ( -0.000000000000000000, 1.000000000000000000, -0.000000000000000000 ) ) ;
#11575 = CARTESIAN_POINT ( 'NONE',  ( -213.3956520262682091, 148.0073597223720583, 9.578254705571842109 ) ) ;
#11576 = DIRECTION ( 'NONE',  ( 0.000000000000000000, 1.000000000000000000, 0.000000000000000000 ) ) ;
#11577 = AXIS2_PLACEMENT_3D ( 'NONE', #7511, #8854, #6410 ) ;
#11578 = CARTESIAN_POINT ( 'NONE',  ( -63.50000000000002842, -179.3058001507315566, 84.88378295107887084 ) ) ;
#11579 = ORIENTED_EDGE ( 'NONE', *, *, #6653, .F. ) ;
#11580 = FACE_BOUND ( 'NONE', #5886, .T. ) ;
#11581 = AXIS2_PLACEMENT_3D ( 'NONE', #10459, #15324, #4522 ) ;
#11582 = ORIENTED_EDGE ( 'NONE', *, *, #11267, .F. ) ;
#11583 = EDGE_CURVE ( 'NONE', #8246, #1098, #10716, .T. ) ;
#11584 = EDGE_CURVE ( 'NONE', #12466, #11151, #8907, .T. ) ;
#11585 = VERTEX_POINT ( 'NONE', #12513 ) ;
#11586 = CYLINDRICAL_SURFACE ( 'NONE', #5297, 1.700000000000007061 ) ;
#11587 = DIRECTION ( 'NONE',  ( -0.000000000000000000, 1.000000000000000000, 1.156482317317871725E-16 ) ) ;
#11588 = EDGE_CURVE ( 'NONE', #10430, #5329, #270, .T. ) ;
#11589 = CARTESIAN_POINT ( 'NONE',  ( -76.00000000000004263, 23.05038067821379499, 35.93956260393299829 ) ) ;
#11590 = CARTESIAN_POINT ( 'NONE',  ( -169.8918728808606886, 123.8447131433307931, 9.392450650342059504 ) ) ;
#11591 = CARTESIAN_POINT ( 'NONE',  ( -222.0684630521171528, 149.3687023665398499, -5.084110969117699774 ) ) ;
#11592 = AXIS2_PLACEMENT_3D ( 'NONE', #11554, #10372, #6519 ) ;
#11593 = AXIS2_PLACEMENT_3D ( 'NONE', #7951, #15103, #13933 ) ;
#11594 = PLANE ( 'NONE',  #10239 ) ;
#11595 = APPLICATION_CONTEXT ( 'automotive_design' ) ;
#11596 = DIRECTION ( 'NONE',  ( 0.000000000000000000, 1.156482317317871478E-16, -1.000000000000000000 ) ) ;
#11597 = CARTESIAN_POINT ( 'NONE',  ( 224.0000000000000853, 22.53993994372673981, 13.00000000000000178 ) ) ;
#11598 = CARTESIAN_POINT ( 'NONE',  ( 190.5000000000000568, -178.9449732516916072, -29.32815825124561471 ) ) ;
#11599 = DIRECTION ( 'NONE',  ( 1.000000000000000000, 0.000000000000000000, 0.000000000000000000 ) ) ;
#11600 = VECTOR ( 'NONE', #15348, 1000.000000000000000 ) ;
#11601 = CARTESIAN_POINT ( 'NONE',  ( 64.00000000000005684, 56.53993994372675047, 15.00000000000070166 ) ) ;
#11602 = ORIENTED_EDGE ( 'NONE', *, *, #3824, .T. ) ;
#11603 = CIRCLE ( 'NONE', #8834, 0.5000000000000004441 ) ;
#11604 = CIRCLE ( 'NONE', #1501, 0.5000000000000004441 ) ;
#11605 = FACE_OUTER_BOUND ( 'NONE', #7602, .T. ) ;
#11606 = ORIENTED_EDGE ( 'NONE', *, *, #7500, .T. ) ;
#11607 = DIRECTION ( 'NONE',  ( 1.000000000000000000, 0.000000000000000000, 0.000000000000000000 ) ) ;
#11608 = DIRECTION ( 'NONE',  ( 1.000000000000000000, 0.000000000000000000, 0.000000000000000000 ) ) ;
#11609 = ORIENTED_EDGE ( 'NONE', *, *, #7899, .T. ) ;
#11610 = CARTESIAN_POINT ( 'NONE',  ( -206.0179204244930702, 148.9258921110169638, 2.500000000000000000 ) ) ;
#11611 = CARTESIAN_POINT ( 'NONE',  ( 190.0000000000000853, -179.3058001507315566, 52.19066787724494816 ) ) ;
#11612 = LINE ( 'NONE', #1813, #1080 ) ;
#11614 = VERTEX_POINT ( 'NONE', #8670 ) ;
#11613 = ADVANCED_FACE ( 'NONE', ( #499 ), #5340, .F. ) ;
#11615 = AXIS2_PLACEMENT_3D ( 'NONE', #14151, #2392, #11792 ) ;
#11616 = CIRCLE ( 'NONE', #4806, 1.699999999999993072 ) ;
#11617 = SHAPE_DEFINITION_REPRESENTATION ( #12541, #5419 ) ;
#11618 = EDGE_LOOP ( 'NONE', ( #14642, #14831, #12774, #15225 ) ) ;
#11619 = CARTESIAN_POINT ( 'NONE',  ( 188.3692075015854357, 39.10978640110493387, -4.508345083535985509 ) ) ;
#11620 = EDGE_CURVE ( 'NONE', #10652, #9742, #11032, .T. ) ;
#11621 = DIRECTION ( 'NONE',  ( 1.000000000000000000, -0.000000000000000000, -0.000000000000000000 ) ) ;
#11622 = ORIENTED_EDGE ( 'NONE', *, *, #11322, .F. ) ;
#11623 = DIRECTION ( 'NONE',  ( -0.000000000000000000, 1.000000000000000000, -0.000000000000000000 ) ) ;
#11624 = CARTESIAN_POINT ( 'NONE',  ( 163.3793289068652257, 15.80605437029538507, -6.370175303308196924 ) ) ;
#11625 = CIRCLE ( 'NONE', #4816, 0.5000000000000004441 ) ;
#11626 = EDGE_LOOP ( 'NONE', ( #14392, #8254 ) ) ;
#11627 = ORIENTED_EDGE ( 'NONE', *, *, #7297, .F. ) ;
#11628 = FACE_OUTER_BOUND ( 'NONE', #14522, .T. ) ;
#11629 = DIRECTION ( 'NONE',  ( 0.000000000000000000, 0.000000000000000000, -1.000000000000000000 ) ) ;
#11630 = AXIS2_PLACEMENT_3D ( 'NONE', #8207, #10322, #5505 ) ;
#11631 = ADVANCED_FACE ( 'NONE', ( #3851 ), #13466, .F. ) ;
#11632 = EDGE_LOOP ( 'NONE', ( #9188, #15172, #3690, #2301 ) ) ;
#11633 = FACE_OUTER_BOUND ( 'NONE', #2822, .T. ) ;
#11634 = CARTESIAN_POINT ( 'NONE',  ( 224.0000000000000853, 59.53993994372674337, 10.00000000000000178 ) ) ;
#11635 = CARTESIAN_POINT ( 'NONE',  ( 6.399999999999999467, 6.613092715395731132E-16, 5.400000000000019007 ) ) ;
#11636 = CARTESIAN_POINT ( 'NONE',  ( -64.00000000000002842, 16.03993994372673981, -3.075184203610571654 ) ) ;
#11637 = LINE ( 'NONE', #11481, #13607 ) ;
#11638 = CIRCLE ( 'NONE', #4561, 1.700000000000007061 ) ;
#11639 = DIRECTION ( 'NONE',  ( 0.000000000000000000, 0.000000000000000000, -1.000000000000000000 ) ) ;
#11640 = COLOUR_RGB ( '', 0.31764706, 0.68627451, 0.89019608) ;
#11641 = ORIENTED_EDGE ( 'NONE', *, *, #12557, .T. ) ;
#11642 = DIRECTION ( 'NONE',  ( 0.000000000000000000, 0.000000000000000000, 1.000000000000000000 ) ) ;
#11643 = CARTESIAN_POINT ( 'NONE',  ( -215.7895908902557380, 152.2252679817794956, -2.963320117457100444 ) ) ;
#11644 = CYLINDRICAL_SURFACE ( 'NONE', #11581, 1.499999999999994227 ) ;
#11645 = ORIENTED_EDGE ( 'NONE', *, *, #14529, .F. ) ;
#11646 = CARTESIAN_POINT ( 'NONE',  ( -220.6443225159919734, 151.9202736894074803, -4.662307221713795968 ) ) ;
#11647 = CARTESIAN_POINT ( 'NONE',  ( 204.3809113867051508, 51.54681031777401756, 0.6364305089822913652 ) ) ;
#11648 = ORIENTED_EDGE ( 'NONE', *, *, #15038, .F. ) ;
#11649 = ADVANCED_FACE ( 'NONE', ( #3201 ), #15339, .F. ) ;
#11651 = EDGE_CURVE ( 'NONE', #12939, #2150, #12215, .T. ) ;
#11650 = EDGE_CURVE ( 'NONE', #3571, #7716, #11980, .T. ) ;
#11652 = CIRCLE ( 'NONE', #10383, 1.700000000000007061 ) ;
#11653 = DIRECTION ( 'NONE',  ( -0.000000000000000000, 1.000000000000000000, 1.156482317317871725E-16 ) ) ;
#11654 = CARTESIAN_POINT ( 'NONE',  ( -63.50000000000002842, -178.6666270497714777, -18.18093594598675011 ) ) ;
#11655 = ADVANCED_FACE ( 'NONE', ( #4457 ), #13221, .F. ) ;
#11656 = CIRCLE ( 'NONE', #10646, 1.699999999999993072 ) ;
#11657 = DIRECTION ( 'NONE',  ( 0.000000000000000000, 0.000000000000000000, 1.000000000000000000 ) ) ;
#11658 = ORIENTED_EDGE ( 'NONE', *, *, #11650, .F. ) ;
#11659 = CARTESIAN_POINT ( 'NONE',  ( -64.00000000000002842, 15.03993994372673804, 38.07518420361041933 ) ) ;
#11660 = ORIENTED_EDGE ( 'NONE', *, *, #3369, .F. ) ;
#11661 = AXIS2_PLACEMENT_3D ( 'NONE', #1928, #2093, #4143 ) ;
#11662 = CARTESIAN_POINT ( 'NONE',  ( -34.79899788034579444, 48.72489408690345414, 7.600000000000002309 ) ) ;
#11663 = CARTESIAN_POINT ( 'NONE',  ( -171.9895241055258168, 125.0924944214600885, 9.516496325551347724 ) ) ;
#11664 = DIRECTION ( 'NONE',  ( 0.000000000000000000, 0.000000000000000000, 1.000000000000000000 ) ) ;
#11665 = FACE_OUTER_BOUND ( 'NONE', #5507, .T. ) ;
#11666 = ORIENTED_EDGE ( 'NONE', *, *, #15038, .T. ) ;
#11667 = CLOSED_SHELL ( 'NONE', ( #1428, #9145, #11549, #12119, #5688, #11613, #14051, #11073, #12741, #14492, #1703, #10904, #13424, #11168, #111, #5849, #6484, #5387, #5326, #1541, #6733, #3246, #10595, #6178, #13637, #10144, #14710, #8289, #3549, #2402, #11874, #15468, #6872, #1579, #3439, #13298, #2232, #262, #11740, #6709, #14433, #2477, #15487, #8828, #14393, #6565, #7947, #9399 ) ) ;
#11668 = CARTESIAN_POINT ( 'NONE',  ( -85.99999999999994316, 64.53993994372673626, 18.50000000000175149 ) ) ;
#11669 = ORIENTED_EDGE ( 'NONE', *, *, #13656, .F. ) ;
#11670 = ORIENTED_EDGE ( 'NONE', *, *, #14145, .T. ) ;
#11671 = CARTESIAN_POINT ( 'NONE',  ( 190.5000000000000568, 19.53993994372674692, -17.50000000000002487 ) ) ;
#11672 = FACE_OUTER_BOUND ( 'NONE', #12808, .T. ) ;
#11673 = DIRECTION ( 'NONE',  ( 5.518327896226365911E-17, 0.9902680687415714722, -0.1391731009600582769 ) ) ;
#11674 = CARTESIAN_POINT ( 'NONE',  ( -170.3246542751710422, 123.0693173402045204, 9.678964735678034614 ) ) ;
#11675 = CARTESIAN_POINT ( 'NONE',  ( -221.6215556288433675, 150.1694071680115883, -2.996691548334699196 ) ) ;
#11676 = ADVANCED_FACE ( 'NONE', ( #3287 ), #4915, .T. ) ;
#11677 = DIRECTION ( 'NONE',  ( -0.000000000000000000, -0.000000000000000000, -1.000000000000000000 ) ) ;
#11678 = LINE ( 'NONE', #3144, #576 ) ;
#11679 = CARTESIAN_POINT ( 'NONE',  ( -151.4086188282879277, 107.2728346664360259, 84.88378295107887084 ) ) ;
#11680 = EDGE_CURVE ( 'NONE', #4447, #7455, #15234, .T. ) ;
#11681 = FACE_BOUND ( 'NONE', #9294, .T. ) ;
#11682 = FACE_OUTER_BOUND ( 'NONE', #1859, .T. ) ;
#11683 = ORIENTED_EDGE ( 'NONE', *, *, #7328, .F. ) ;
#11684 = SHAPE_REPRESENTATION_RELATIONSHIP ( 'NONE' , 'NONE' ,  #556, #3584 ) ;
#11685 = ORIENTED_EDGE ( 'NONE', *, *, #5573, .T. ) ;
#11686 = DIRECTION ( 'NONE',  ( 0.6130913241491352528, 0.7900120431063439863, -6.390853288715847897E-17 ) ) ;
#11687 = AXIS2_PLACEMENT_3D ( 'NONE', #12924, #3218, #8140 ) ;
#11688 = ORIENTED_EDGE ( 'NONE', *, *, #9331, .T. ) ;
#11689 = DIRECTION ( 'NONE',  ( 1.000000000000000000, 0.000000000000000000, 0.000000000000000000 ) ) ;
#11690 = CARTESIAN_POINT ( 'NONE',  ( -136.1405586187959784, 108.3975249866138597, 5.000000000000000000 ) ) ;
#11691 = PRODUCT_DEFINITION_SHAPE ( 'NONE', 'NONE',  #5848 ) ;
#11692 = CIRCLE ( 'NONE', #11437, 7.499999999999999112 ) ;
#11693 = PLANE ( 'NONE',  #5879 ) ;
#11694 = ORIENTED_EDGE ( 'NONE', *, *, #2540, .T. ) ;
#11695 = EDGE_CURVE ( 'NONE', #5784, #9446, #6440, .T. ) ;
#11696 = B_SPLINE_CURVE_WITH_KNOTS ( 'NONE', 3,
 ( #8709, #1665, #5384, #10205, #2865, #6424, #1509, #13501, #14763, #13738, #14995, #3956, #7687, #6501, #8781, #5299, #14836, #13660 ),
 .UNSPECIFIED., .F., .F.,
 ( 4, 2, 2, 2, 2, 2, 2, 2, 4 ),
 ( 0.003229178684347155416, 0.003627155556181209124, 0.004025132428015262831, 0.004423109299849316105, 0.004821086171683369379, 0.005219063043517423520, 0.005617039915351476793, 0.006015016787185530067, 0.006412993659019584208 ),
 .UNSPECIFIED. ) ;
#11697 = VERTEX_POINT ( 'NONE', #7885 ) ;
#11698 = AXIS2_PLACEMENT_3D ( 'NONE', #10104, #2844, #2922 ) ;
#11699 = PRESENTATION_STYLE_ASSIGNMENT (( #14939 ) ) ;
#11700 = VERTEX_POINT ( 'NONE', #5656 ) ;
#11701 = FACE_OUTER_BOUND ( 'NONE', #15054, .T. ) ;
#11702 = CIRCLE ( 'NONE', #11452, 0.5000000000000004441 ) ;
#11703 = PLANE ( 'NONE',  #9866 ) ;
#11704 = FACE_OUTER_BOUND ( 'NONE', #11976, .T. ) ;
#11705 = ORIENTED_EDGE ( 'NONE', *, *, #13012, .F. ) ;
#11706 = ORIENTED_EDGE ( 'NONE', *, *, #14989, .T. ) ;
#11707 = CARTESIAN_POINT ( 'NONE',  ( 169.0043059057019832, 61.25683321636181233, 10.00000000000000178 ) ) ;
#11708 = CYLINDRICAL_SURFACE ( 'NONE', #1786, 0.5000000000000004441 ) ;
#11709 = CIRCLE ( 'NONE', #4901, 1.499999999999994449 ) ;
#11710 = ORIENTED_EDGE ( 'NONE', *, *, #2684, .F. ) ;
#11711 = CARTESIAN_POINT ( 'NONE',  ( 5.799999999999999822, 0.000000000000000000, 8.000000000000007105 ) ) ;
#11712 = AXIS2_PLACEMENT_3D ( 'NONE', #2703, #13265, #7524 ) ;
#11713 = FACE_OUTER_BOUND ( 'NONE', #13886, .T. ) ;
#11714 = FACE_OUTER_BOUND ( 'NONE', #3448, .T. ) ;
#11715 = VECTOR ( 'NONE', #6414, 1000.000000000000000 ) ;
#11716 = ADVANCED_FACE ( 'NONE', ( #4543 ), #2975, .F. ) ;
#11717 = DIRECTION ( 'NONE',  ( -0.000000000000000000, 1.000000000000000000, -0.000000000000000000 ) ) ;
#11718 = EDGE_LOOP ( 'NONE', ( #8715, #8435, #7091, #2333, #1020, #11388 ) ) ;
#11719 = CARTESIAN_POINT ( 'NONE',  ( -215.1139964504661464, 145.4140256597743814, 2.431557144026069928 ) ) ;
#11720 = CARTESIAN_POINT ( 'NONE',  ( -206.0179204244930702, 148.9258921110169638, 2.500000000000000000 ) ) ;
#11721 = CYLINDRICAL_SURFACE ( 'NONE', #9066, 1.499999999999997780 ) ;
#11722 = VERTEX_POINT ( 'NONE', #12591 ) ;
#11723 = CARTESIAN_POINT ( 'NONE',  ( -224.7459018048070050, 144.5716505541534218, -3.023257939496649449 ) ) ;
#11724 = CARTESIAN_POINT ( 'NONE',  ( 207.4341467637200651, 31.47497422714618764, -9.505705820141434614 ) ) ;
#11725 = ORIENTED_EDGE ( 'NONE', *, *, #15101, .F. ) ;
#11726 = CARTESIAN_POINT ( 'NONE',  ( 177.5000000000000853, 17.53993994372673981, -17.50000000000002487 ) ) ;
#11727 = CARTESIAN_POINT ( 'NONE',  ( 17.41029453487719181, 40.04259805664093363, 10.00000000000000178 ) ) ;
#11728 = EDGE_CURVE ( 'NONE', #11157, #10552, #5418, .T. ) ;
#11729 = FACE_OUTER_BOUND ( 'NONE', #8538, .T. ) ;
#11730 = VECTOR ( 'NONE', #7002, 1000.000000000000000 ) ;
#11731 = VERTEX_POINT ( 'NONE', #12667 ) ;
#11732 = EDGE_CURVE ( 'NONE', #11344, #10124, #3650, .T. ) ;
#11733 = CARTESIAN_POINT ( 'NONE',  ( 178.0000000000000853, 15.10952649420676686, 25.44255979523916977 ) ) ;
#11734 = EDGE_CURVE ( 'NONE', #13543, #13999, #8703, .T. ) ;
#11735 = CARTESIAN_POINT ( 'NONE',  ( 194.8381067511959372, 47.88228248201940573, -3.436395123936771601 ) ) ;
#11736 = ORIENTED_EDGE ( 'NONE', *, *, #7900, .T. ) ;
#11737 = CARTESIAN_POINT ( 'NONE',  ( -99.68324453533686835, 80.15913712344708131, 10.00000000000000178 ) ) ;
#11738 = CARTESIAN_POINT ( 'NONE',  ( -192.4722482905459344, 130.7344553107722902, 9.577123744044227394 ) ) ;
#11739 = DIRECTION ( 'NONE',  ( -1.000000000000000000, 0.000000000000000000, 0.000000000000000000 ) ) ;
#11740 = ADVANCED_FACE ( 'NONE', ( #6767 ), #741, .F. ) ;
#11741 = CARTESIAN_POINT ( 'NONE',  ( -70.00000000000000000, 17.53993994372673981, -13.99999999999999289 ) ) ;
#11742 = DIRECTION ( 'NONE',  ( -3.965082230804130220E-16, -4.956352788505162775E-17, 1.000000000000000000 ) ) ;
#11743 = VECTOR ( 'NONE', #15461, 1000.000000000000000 ) ;
#11744 = VERTEX_POINT ( 'NONE', #6850 ) ;
#11745 = ORIENTED_EDGE ( 'NONE', *, *, #1608, .F. ) ;
#11746 = CARTESIAN_POINT ( 'NONE',  ( -70.00000000000000000, 17.53993994372673271, 47.49999999999997868 ) ) ;
#11747 = CARTESIAN_POINT ( 'NONE',  ( 0.000000000000000000, -2.775557561562891351E-14, -8.000000000000007105 ) ) ;
#11748 = DIRECTION ( 'NONE',  ( -0.7071067811865965336, 8.659560562355533132E-17, 0.7071067811864985009 ) ) ;
#11749 = CARTESIAN_POINT ( 'NONE',  ( -167.7990583880505824, 127.5943188236592363, 2.500000001005440620 ) ) ;
#11750 = CARTESIAN_POINT ( 'NONE',  ( -222.0498794291082163, 149.4019978443419348, -3.065875947492658238 ) ) ;
#11751 = CARTESIAN_POINT ( 'NONE',  ( -223.6145774380523505, 142.0129443944823606, 2.393984899497048513 ) ) ;
#11752 = AXIS2_PLACEMENT_3D ( 'NONE', #4582, #6967, #3558 ) ;
#11753 = ADVANCED_FACE ( 'NONE', ( #5583 ), #10391, .T. ) ;
#11754 = EDGE_CURVE ( 'NONE', #6332, #10430, #872, .T. ) ;
#11755 = DIRECTION ( 'NONE',  ( 1.000000000000000000, 0.000000000000000000, 0.000000000000000000 ) ) ;
#11756 = FACE_BOUND ( 'NONE', #2790, .T. ) ;
#11757 = DIRECTION ( 'NONE',  ( 0.000000000000000000, 4.956352788505162775E-17, -1.000000000000000000 ) ) ;
#11758 = LINE ( 'NONE', #10809, #4321 ) ;
#11759 = ORIENTED_EDGE ( 'NONE', *, *, #3443, .F. ) ;
#11760 = ORIENTED_EDGE ( 'NONE', *, *, #1025, .F. ) ;
#11761 = DIRECTION ( 'NONE',  ( 1.000000000000000000, -2.751328491981765035E-32, 3.965082230804130220E-16 ) ) ;
#11762 = LINE ( 'NONE', #1165, #13905 ) ;
#11763 = EDGE_LOOP ( 'NONE', ( #10692, #8889, #4666, #7909 ) ) ;
#11764 = CARTESIAN_POINT ( 'NONE',  ( -34.79899788034579444, 48.72489408690345414, 7.600000000000002309 ) ) ;
#11765 = CARTESIAN_POINT ( 'NONE',  ( 164.0000000000000568, 64.51493994372674479, 15.00000000000000355 ) ) ;
#11766 = AXIS2_PLACEMENT_3D ( 'NONE', #9715, #1169, #7202 ) ;
#11767 = EDGE_CURVE ( 'NONE', #11836, #5551, #8121, .T. ) ;
#11768 = VECTOR ( 'NONE', #8901, 1000.000000000000000 ) ;
#11769 = ORIENTED_EDGE ( 'NONE', *, *, #2189, .T. ) ;
#11770 = CONTEXT_DEPENDENT_SHAPE_REPRESENTATION ( #8672, #9036 ) ;
#11771 = ORIENTED_EDGE ( 'NONE', *, *, #13444, .T. ) ;
#11772 = CARTESIAN_POINT ( 'NONE',  ( 190.6749524420355328, 33.64372802412135144, -4.260924496400990691 ) ) ;
#11773 = CARTESIAN_POINT ( 'NONE',  ( 0.4973051450695281650, -3.866309095700691145, 8.000000000000007105 ) ) ;
#11774 = ORIENTED_EDGE ( 'NONE', *, *, #2683, .F. ) ;
#11775 = CYLINDRICAL_SURFACE ( 'NONE', #3675, 7.499999999999999112 ) ;
#11776 = CARTESIAN_POINT ( 'NONE',  ( -155.6477983077465410, 110.1970436846185066, 9.719846845941789937 ) ) ;
#11777 = CARTESIAN_POINT ( 'NONE',  ( 114.0000000000000568, 64.53993994372673626, 15.00000000000035172 ) ) ;
#11778 = ORIENTED_EDGE ( 'NONE', *, *, #1290, .T. ) ;
#11779 = EDGE_LOOP ( 'NONE', ( #3954, #3513, #11759, #14782, #14778 ) ) ;
#11780 = DIRECTION ( 'NONE',  ( 1.000000000000000000, 0.000000000000000000, 0.000000000000000000 ) ) ;
#11781 = FACE_OUTER_BOUND ( 'NONE', #8489, .T. ) ;
#11782 = EDGE_LOOP ( 'NONE', ( #15577, #9478, #7837, #2052 ) ) ;
#11783 = DIRECTION ( 'NONE',  ( -1.000000000000000000, 0.000000000000000000, 0.000000000000000000 ) ) ;
#11784 = CARTESIAN_POINT ( 'NONE',  ( 178.0000000000000853, -178.6666270497714777, -18.18093594598673945 ) ) ;
#11785 = ADVANCED_FACE ( 'NONE', ( #1139 ), #8272, .F. ) ;
#11786 = DIRECTION ( 'NONE',  ( -0.000000000000000000, 1.000000000000000000, 1.156482317317871725E-16 ) ) ;
#11787 = ORIENTED_EDGE ( 'NONE', *, *, #8624, .T. ) ;
#11788 = ORIENTED_EDGE ( 'NONE', *, *, #1311, .F. ) ;
#11789 = SURFACE_STYLE_USAGE ( .BOTH. , #6984 ) ;
#11790 = VERTEX_POINT ( 'NONE', #9680 ) ;
#11791 = CARTESIAN_POINT ( 'NONE',  ( 190.5000000000000568, 14.97035339324670922, -2.580050169239785696 ) ) ;
#11792 = DIRECTION ( 'NONE',  ( -0.4873681696970831312, -0.8731965799097676229, 0.000000000000000000 ) ) ;
#11793 = CARTESIAN_POINT ( 'NONE',  ( 64.00000000000005684, 59.53993994372674337, 15.00000000000070166 ) ) ;
#11794 = ORIENTED_EDGE ( 'NONE', *, *, #6142, .T. ) ;
#11795 = CARTESIAN_POINT ( 'NONE',  ( -209.2375803003894532, 133.3242992996629539, -0.4555467707853204096 ) ) ;
#11796 = UNCERTAINTY_MEASURE_WITH_UNIT (LENGTH_MEASURE( 1.000000000000000082E-05 ), #4919, 'distance_accuracy_value', 'NONE');
#11797 = CARTESIAN_POINT ( 'NONE',  ( 203.8319104552679448, 51.73948369304471839, -2.483607112462900446 ) ) ;
#11798 = CIRCLE ( 'NONE', #8286, 1.700000000000007061 ) ;
#11799 = ORIENTED_EDGE ( 'NONE', *, *, #12284, .T. ) ;
#11800 = CARTESIAN_POINT ( 'NONE',  ( 5.196152422706632024, 9.000000000000003553, 0.000000000000000000 ) ) ;
#11801 = CARTESIAN_POINT ( 'NONE',  ( -64.00000000000002842, -178.8753867012115961, -29.82329228561640022 ) ) ;
#11802 = DIRECTION ( 'NONE',  ( -1.000000000000000000, 0.000000000000000000, 0.000000000000000000 ) ) ;
#11803 = CIRCLE ( 'NONE', #13808, 1.699999999999994849 ) ;
#11804 = ORIENTED_EDGE ( 'NONE', *, *, #4277, .F. ) ;
#11805 = AXIS2_PLACEMENT_3D ( 'NONE', #11624, #6970, #4659 ) ;
#11806 = EDGE_CURVE ( 'NONE', #935, #7752, #4862, .T. ) ;
#11807 = AXIS2_PLACEMENT_3D ( 'NONE', #13619, #5035, #2508 ) ;
#11808 = DIRECTION ( 'NONE',  ( 0.000000000000000000, 0.000000000000000000, 0.9999999999999998890 ) ) ;
#11809 = PRESENTATION_STYLE_ASSIGNMENT (( #11887 ) ) ;
#11810 = CARTESIAN_POINT ( 'NONE',  ( 191.3767946852191528, 39.76267059705192253, -4.365329018565075714 ) ) ;
#11811 = ORIENTED_EDGE ( 'NONE', *, *, #9302, .T. ) ;
#11812 = CARTESIAN_POINT ( 'NONE',  ( 200.1062858801516597, 40.86394065090267702, 10.00000000000000000 ) ) ;
#11813 = CARTESIAN_POINT ( 'NONE',  ( -221.5559209476002991, 141.9078401207188449, -0.4555467707853290138 ) ) ;
#11814 = CARTESIAN_POINT ( 'NONE',  ( 5.799999999999999822, 4.618802153516981868, -7.999999999999979572 ) ) ;
#11815 = CYLINDRICAL_SURFACE ( 'NONE', #6561, 1.699999999999994849 ) ;
#11816 = LINE ( 'NONE', #4225, #7357 ) ;
#11817 = CIRCLE ( 'NONE', #10048, 1.700000000000007061 ) ;
#11818 = EDGE_LOOP ( 'NONE', ( #3193, #1363, #13542, #7329, #13365, #10685 ) ) ;
#11819 = ORIENTED_EDGE ( 'NONE', *, *, #6481, .T. ) ;
#11820 = DIRECTION ( 'NONE',  ( 1.000000000000000000, 0.000000000000000000, 0.000000000000000000 ) ) ;
#11821 = CARTESIAN_POINT ( 'NONE',  ( -1.273212868926705820E-14, 0.3912769056150044999, -7.999999999999981348 ) ) ;
#11822 = AXIS2_PLACEMENT_3D ( 'NONE', #9125, #571, #5409 ) ;
#11823 = EDGE_CURVE ( 'NONE', #11943, #13871, #8956, .T. ) ;
#11824 = CARTESIAN_POINT ( 'NONE',  ( -151.4086188282879277, 107.2728346664360259, 5.000000000000004441 ) ) ;
#11825 = DIRECTION ( 'NONE',  ( 0.000000000000000000, -0.000000000000000000, 1.000000000000000000 ) ) ;
#11826 = CARTESIAN_POINT ( 'NONE',  ( -221.7378436215748820, 145.6645920127244835, -4.300707049757050093 ) ) ;
#11827 = LINE ( 'NONE', #13482, #8432 ) ;
#11828 = DIRECTION ( 'NONE',  ( 1.000000000000000000, 0.000000000000000000, 0.000000000000000000 ) ) ;
#11829 = VECTOR ( 'NONE', #15467, 1000.000000000000000 ) ;
#11830 = LINE ( 'NONE', #4715, #1866 ) ;
#11831 = CIRCLE ( 'NONE', #2505, 1.000000000000000888 ) ;
#11832 = CARTESIAN_POINT ( 'NONE',  ( -172.3582205330567945, 130.1389812296867774, 2.500000000525777644 ) ) ;
#11833 = CARTESIAN_POINT ( 'NONE',  ( 181.4384305232223369, 82.69763993231136112, 5.000000000000000000 ) ) ;
#11834 = CARTESIAN_POINT ( 'NONE',  ( -157.8787660911425803, 118.6941998492684149, 0.000000000000000000 ) ) ;
#11835 = VERTEX_POINT ( 'NONE', #4695 ) ;
#11836 = VERTEX_POINT ( 'NONE', #9517 ) ;
#11837 = CYLINDRICAL_SURFACE ( 'NONE', #678, 1.700000000000007061 ) ;
#11838 = CARTESIAN_POINT ( 'NONE',  ( -216.6986482686336331, 154.8858946472299465, 2.630718524060158714 ) ) ;
#11839 = ORIENTED_EDGE ( 'NONE', *, *, #4078, .T. ) ;
#11840 = EDGE_CURVE ( 'NONE', #9838, #5937, #14973, .T. ) ;
#11841 = VECTOR ( 'NONE', #9747, 1000.000000000000000 ) ;
#11842 = CARTESIAN_POINT ( 'NONE',  ( -216.6980668629938123, 154.8869363267023687, 2.500000000158653091 ) ) ;
#11843 = CARTESIAN_POINT ( 'NONE',  ( 0.000000000000000000, 0.000000000000000000, 18.00000000000000355 ) ) ;
#11845 = EDGE_CURVE ( 'NONE', #12599, #12968, #14474, .T. ) ;
#11844 = EDGE_CURVE ( 'NONE', #3979, #5229, #5163, .T. ) ;
#11846 = AXIS2_PLACEMENT_3D ( 'NONE', #8422, #3739, #9830 ) ;
#11847 = CONICAL_SURFACE ( 'NONE', #7028, 3.525000000000000355, 0.7853981633973787790 ) ;
#11848 = ORIENTED_EDGE ( 'NONE', *, *, #5953, .T. ) ;
#11849 = VECTOR ( 'NONE', #12516, 1000.000000000000000 ) ;
#11850 = ORIENTED_EDGE ( 'NONE', *, *, #11922, .T. ) ;
#11851 = AXIS2_PLACEMENT_3D ( 'NONE', #876, #7201, #11999 ) ;
#11852 = CARTESIAN_POINT ( 'NONE',  ( 190.7182813446581235, 33.54593944905032998, -7.256469109801526152 ) ) ;
#11853 = CARTESIAN_POINT ( 'NONE',  ( 14.00000000000004086, 56.53993994372675047, 13.30000000000105231 ) ) ;
#11854 = ORIENTED_EDGE ( 'NONE', *, *, #3332, .F. ) ;
#11855 = DIRECTION ( 'NONE',  ( 0.4873681696970814659, 0.8731965799097686221, 0.000000000000000000 ) ) ;
#11856 = FACE_OUTER_BOUND ( 'NONE', #5665, .T. ) ;
#11857 = ORIENTED_EDGE ( 'NONE', *, *, #917, .T. ) ;
#11858 = VERTEX_POINT ( 'NONE', #2335 ) ;
#11859 = CARTESIAN_POINT ( 'NONE',  ( 184.0000000000000568, -179.3058001507315566, 77.95141194869098911 ) ) ;
#11860 = FACE_OUTER_BOUND ( 'NONE', #10192, .T. ) ;
#11861 = ORIENTED_EDGE ( 'NONE', *, *, #12028, .T. ) ;
#11862 = CARTESIAN_POINT ( 'NONE',  ( -152.3840324909117214, 107.0166450474691260, 9.325089004845759533 ) ) ;
#11863 = CYLINDRICAL_SURFACE ( 'NONE', #12847, 1.000000000000000888 ) ;
#11864 = AXIS2_PLACEMENT_3D ( 'NONE', #5778, #8010, #14141 ) ;
#11865 = AXIS2_PLACEMENT_3D ( 'NONE', #10415, #3309, #8144 ) ;
#11866 = CIRCLE ( 'NONE', #12360, 4.999999999999990230 ) ;
#11867 = DIRECTION ( 'NONE',  ( 0.000000000000000000, 0.000000000000000000, -1.000000000000000000 ) ) ;
#11868 = ORIENTED_EDGE ( 'NONE', *, *, #15474, .F. ) ;
#11869 = LINE ( 'NONE', #3343, #993 ) ;
#11870 = VECTOR ( 'NONE', #15292, 1000.000000000000000 ) ;
#11871 = ORIENTED_EDGE ( 'NONE', *, *, #15290, .T. ) ;
#11872 = CARTESIAN_POINT ( 'NONE',  ( -10.39230484541326582, 4.570335331080236228E-16, 5.000000000000000000 ) ) ;
#11873 = AXIS2_PLACEMENT_3D ( 'NONE', #6304, #2017, #3133 ) ;
#11874 = ADVANCED_FACE ( 'NONE', ( #14316 ), #14398, .F. ) ;
#11875 = CARTESIAN_POINT ( 'NONE',  ( -201.8658614229783268, 146.6084512934502584, 2.500000000000000000 ) ) ;
#11876 = SHAPE_REPRESENTATION ( 'hex bolt gradeb_iso_ISO 4015 - M3 x 20 x 12-N', ( #12337 ), #5251 ) ;
#11877 = DIRECTION ( 'NONE',  ( 1.000000000000000000, 0.000000000000000000, 0.000000000000000000 ) ) ;
#11878 = ORIENTED_EDGE ( 'NONE', *, *, #13818, .T. ) ;
#11879 = CARTESIAN_POINT ( 'NONE',  ( -182.6467173238959560, 123.4549944991208292, -4.642206099735001423 ) ) ;
#11880 = CARTESIAN_POINT ( 'NONE',  ( 207.3850704934720284, 31.45434786795649984, -6.508326106789642296 ) ) ;
#11881 = ORIENTED_EDGE ( 'NONE', *, *, #4730, .T. ) ;
#11882 = CARTESIAN_POINT ( 'NONE',  ( 114.0000000000000568, 64.53993994372673626, 16.70000000000034746 ) ) ;
#11883 = CARTESIAN_POINT ( 'NONE',  ( 200.1062858801516597, 40.86394065090267702, 0.000000000000000000 ) ) ;
#11884 = CARTESIAN_POINT ( 'NONE',  ( -152.4086188282879277, 107.0149490162102808, -4.459856507254708724 ) ) ;
#11885 = VECTOR ( 'NONE', #792, 1000.000000000000000 ) ;
#11886 = AXIS2_PLACEMENT_3D ( 'NONE', #781, #8727, #12495 ) ;
#11887 = SURFACE_STYLE_USAGE ( .BOTH. , #7239 ) ;
#11888 = CARTESIAN_POINT ( 'NONE',  ( 205.5140042898306660, 47.80506208259531320, -5.491262609045910459 ) ) ;
#11889 = ORIENTED_EDGE ( 'NONE', *, *, #5899, .F. ) ;
#11890 = DIRECTION ( 'NONE',  ( 1.000000000000000000, 0.000000000000000000, 0.000000000000000000 ) ) ;
#11891 = CARTESIAN_POINT ( 'NONE',  ( -173.9416064256852508, 115.8726071073731987, 1.253181679794994174 ) ) ;
#11892 = DIRECTION ( 'NONE',  ( -0.000000000000000000, 1.000000000000000000, -0.000000000000000000 ) ) ;
#11893 = DIRECTION ( 'NONE',  ( -0.000000000000000000, 1.000000000000000000, -0.000000000000000000 ) ) ;
#11895 = FACE_BOUND ( 'NONE', #3727, .T. ) ;
#11894 = VECTOR ( 'NONE', #5290, 1000.000000000000000 ) ;
#11896 = ORIENTED_EDGE ( 'NONE', *, *, #8483, .T. ) ;
#11897 = ORIENTED_EDGE ( 'NONE', *, *, #10794, .F. ) ;
#11898 = CARTESIAN_POINT ( 'NONE',  ( 205.4699394944333051, 33.88363592193200446, -7.930995773285529182 ) ) ;
#11899 = LINE ( 'NONE', #9528, #9581 ) ;
#11900 = EDGE_CURVE ( 'NONE', #9167, #8877, #3363, .T. ) ;
#11901 = CARTESIAN_POINT ( 'NONE',  ( 190.5000000000000853, -178.6666270497714777, 53.18093594598651919 ) ) ;
#11902 = PLANE ( 'NONE',  #387 ) ;
#11903 = CARTESIAN_POINT ( 'NONE',  ( -222.8935454358862387, 147.8904377599758391, -2.724937377524569104 ) ) ;
#11904 = CARTESIAN_POINT ( 'NONE',  ( -223.4402560244223821, 142.3745948123178664, 4.936224999423321158 ) ) ;
#11905 = DIRECTION ( 'NONE',  ( 0.000000000000000000, 0.000000000000000000, -1.000000000000000000 ) ) ;
#11906 = AXIS2_PLACEMENT_3D ( 'NONE', #6790, #12690, #680 ) ;
#11907 = DIRECTION ( 'NONE',  ( 1.000000000000000000, 0.000000000000000000, 0.000000000000000000 ) ) ;
#11908 = EDGE_CURVE ( 'NONE', #10751, #14668, #11483, .T. ) ;
#11909 = DIRECTION ( 'NONE',  ( -0.000000000000000000, 1.000000000000000000, -0.000000000000000000 ) ) ;
#11910 = CARTESIAN_POINT ( 'NONE',  ( -70.00000000000000000, 17.53993994372673271, 47.49999999999997868 ) ) ;
#11911 = FACE_OUTER_BOUND ( 'NONE', #10222, .T. ) ;
#11912 = ORIENTED_EDGE ( 'NONE', *, *, #4226, .T. ) ;
#11913 =( NAMED_UNIT ( * ) SI_UNIT ( $, .STERADIAN. ) SOLID_ANGLE_UNIT ( ) );
#11914 = ORIENTED_EDGE ( 'NONE', *, *, #3154, .T. ) ;
#11915 = DIRECTION ( 'NONE',  ( -0.000000000000000000, -0.000000000000000000, 1.000000000000000000 ) ) ;
#11916 = LINE ( 'NONE', #10815, #14403 ) ;
#11917 = DIRECTION ( 'NONE',  ( 0.6130913241491352528, 0.7900120431063439863, -6.390853288715847897E-17 ) ) ;
#11918 = FACE_OUTER_BOUND ( 'NONE', #12675, .T. ) ;
#11920 = CLOSED_SHELL ( 'NONE', ( #13102, #6801, #4704, #14904, #3691, #691, #10116, #12724, #2116, #8563, #15434, #7326, #9160, #4397, #14198, #2968, #1506, #365, #15055, #1041, #2842, #2820, #13540, #6053, #15490, #5203, #8134, #13623, #4958, #9357, #607, #14984, #5275, #2019, #3211, #8515, #7287, #10715, #8195, #7478, #14759, #5868, #8383, #190, #13745, #3725, #12002, #4991, #2111, #6497, #10158, #9789, #9439, #5347, #12588, #934, #5933, #1399, #14823, #4336, #11060, #7101, #6246, #7160, #9259, #676, #5115, #10941, #9972, #14278, #6376, #11753, #5130, #13464, #11649, #8992 ) ) ;
#11919 = AXIS2_PLACEMENT_3D ( 'NONE', #1420, #4177, #5379 ) ;
#11921 = DIRECTION ( 'NONE',  ( 0.000000000000000000, 1.000000000000000000, 6.938893903907227145E-17 ) ) ;
#11923 = VERTEX_POINT ( 'NONE', #10785 ) ;
#11922 = EDGE_CURVE ( 'NONE', #1631, #552, #5966, .T. ) ;
#11924 = ITEM_DEFINED_TRANSFORMATION ( 'NONE', 'NONE', #15319,  #12337 ) ;
#11925 = VERTEX_POINT ( 'NONE', #12038 ) ;
#11926 = EDGE_CURVE ( 'NONE', #7344, #6077, #3515, .T. ) ;
#11927 = EDGE_CURVE ( 'NONE', #8811, #13295, #5808, .T. ) ;
#11928 = CARTESIAN_POINT ( 'NONE',  ( -76.50000000000001421, -179.8058001507315566, -51.45141194869120227 ) ) ;
#11929 = ORIENTED_EDGE ( 'NONE', *, *, #7863, .T. ) ;
#11930 = VECTOR ( 'NONE', #10505, 1000.000000000000000 ) ;
#11931 = CARTESIAN_POINT ( 'NONE',  ( -168.8345777152483151, 119.5835126658289909, 2.431557144026069928 ) ) ;
#11932 = CARTESIAN_POINT ( 'NONE',  ( -225.4016773603011927, 143.3967257069427887, 5.447776948886904336 ) ) ;
#11933 = ORIENTED_EDGE ( 'NONE', *, *, #4198, .F. ) ;
#11934 = EDGE_CURVE ( 'NONE', #1467, #11722, #1065, .T. ) ;
#11935 = VERTEX_POINT ( 'NONE', #15420 ) ;
#11936 = DIRECTION ( 'NONE',  ( 1.000000000000000000, 0.000000000000000000, 0.000000000000000000 ) ) ;
#11937 = CARTESIAN_POINT ( 'NONE',  ( 177.5000000000000853, 19.53993994372674692, -17.50000000000002487 ) ) ;
#11938 = EDGE_LOOP ( 'NONE', ( #13233, #12785, #4946, #3407 ) ) ;
#11939 = CARTESIAN_POINT ( 'NONE',  ( -152.0230500315369397, 106.4726074349910760, 9.188529295497623650 ) ) ;
#11940 = DIRECTION ( 'NONE',  ( 0.000000000000000000, -1.000000000000000000, 0.000000000000000000 ) ) ;
#11941 = DIRECTION ( 'NONE',  ( 0.8731965799097684000, -0.4873681696970819655, 0.000000000000000000 ) ) ;
#11942 = CONICAL_SURFACE ( 'NONE', #5133, 3.525000000000000355, 0.7853981633975176679 ) ;
#11943 = VERTEX_POINT ( 'NONE', #8503 ) ;
#11944 = EDGE_CURVE ( 'NONE', #3832, #2866, #8352, .T. ) ;
#11945 = CIRCLE ( 'NONE', #8423, 1.000000000000000888 ) ;
#11946 = PLANE ( 'NONE',  #4015 ) ;
#11947 = ADVANCED_FACE ( 'NONE', ( #2487, #6127 ), #2172, .F. ) ;
#11948 = LINE ( 'NONE', #12170, #9533 ) ;
#11949 = VERTEX_POINT ( 'NONE', #4619 ) ;
#11950 = DIRECTION ( 'NONE',  ( 0.000000000000000000, 0.000000000000000000, -1.000000000000000000 ) ) ;
#11951 = CARTESIAN_POINT ( 'NONE',  ( -185.2055264765504887, 137.3096093875189467, 2.500000000000000000 ) ) ;
#11952 = FACE_OUTER_BOUND ( 'NONE', #15145, .T. ) ;
#11953 = ORIENTED_EDGE ( 'NONE', *, *, #8671, .F. ) ;
#11954 = ORIENTED_EDGE ( 'NONE', *, *, #6481, .F. ) ;
#11955 = CARTESIAN_POINT ( 'NONE',  ( -185.2011473888584874, 137.3174552105199666, 1.515441477536283887 ) ) ;
#11956 = CARTESIAN_POINT ( 'NONE',  ( 205.5291621427655002, 33.93354315402728361, -9.500001906449378808 ) ) ;
#11957 = ORIENTED_EDGE ( 'NONE', *, *, #11002, .F. ) ;
#11958 = AXIS2_PLACEMENT_3D ( 'NONE', #13852, #3047, #3914 ) ;
#11959 = LINE ( 'NONE', #11882, #5031 ) ;
#11960 = DIRECTION ( 'NONE',  ( 0.000000000000000000, -1.000000000000000000, 0.000000000000000000 ) ) ;
#11961 = CARTESIAN_POINT ( 'NONE',  ( -70.00000000000000000, -181.3058001507315566, 76.45141194869098911 ) ) ;
#11962 = EDGE_CURVE ( 'NONE', #14876, #13381, #4516, .T. ) ;
#11963 = EDGE_LOOP ( 'NONE', ( #8297, #1817, #6401, #12324 ) ) ;
#11964 = DIRECTION ( 'NONE',  ( 0.000000000000000000, 0.000000000000000000, -1.000000000000000000 ) ) ;
#11965 = AXIS2_PLACEMENT_3D ( 'NONE', #9773, #14565, #3768 ) ;
#11966 = CARTESIAN_POINT ( 'NONE',  ( 0.01688885742775080370, 6.535341423375568226, -4.680456609903959730 ) ) ;
#11967 = CARTESIAN_POINT ( 'NONE',  ( 203.2140370934807834, 48.77700970988914264, -0.9247215889056725757 ) ) ;
#11968 = VERTEX_POINT ( 'NONE', #7548 ) ;
#11969 = FACE_OUTER_BOUND ( 'NONE', #1102, .T. ) ;
#11970 = DIRECTION ( 'NONE',  ( 0.000000000000000000, 0.000000000000000000, 1.000000000000000000 ) ) ;
#11971 = CARTESIAN_POINT ( 'NONE',  ( -191.3393351389284192, 126.0399454915928317, 5.434137442415923225 ) ) ;
#11972 = FACE_OUTER_BOUND ( 'NONE', #210, .T. ) ;
#11973 = FACE_OUTER_BOUND ( 'NONE', #907, .T. ) ;
#11974 = CARTESIAN_POINT ( 'NONE',  ( -214.7423002846986151, 145.5292334337732711, 10.16010209732751335 ) ) ;
#11975 = CARTESIAN_POINT ( 'NONE',  ( 207.1325720688761294, 35.61275714886660637, -4.804596322733623914 ) ) ;
#11976 = EDGE_LOOP ( 'NONE', ( #6135, #13047, #2237, #14818 ) ) ;
#11977 = VERTEX_POINT ( 'NONE', #5241 ) ;
#11978 = CARTESIAN_POINT ( 'NONE',  ( -182.0948474510348092, 118.3958639477576043, 2.363114587883560436 ) ) ;
#11979 = FACE_OUTER_BOUND ( 'NONE', #6740, .T. ) ;
#11980 = CIRCLE ( 'NONE', #2643, 1.499999999999994449 ) ;
#11981 = CARTESIAN_POINT ( 'NONE',  ( 0.4988340113715870050, 3.871605243926933504, 8.000000000000007105 ) ) ;
#11982 = DIRECTION ( 'NONE',  ( 0.000000000000000000, 0.000000000000000000, 1.000000000000000000 ) ) ;
#11983 = EDGE_CURVE ( 'NONE', #13122, #14293, #4151, .T. ) ;
#11984 = CARTESIAN_POINT ( 'NONE',  ( -70.00000000000000000, -201.3058001507315566, 76.45141194869098911 ) ) ;
#11985 = ADVANCED_FACE ( 'NONE', ( #11097 ), #252, .F. ) ;
#11986 = CARTESIAN_POINT ( 'NONE',  ( -217.1827905065508446, 154.0535767968314644, 6.164366753867413173 ) ) ;
#11987 = DIRECTION ( 'NONE',  ( -0.000000000000000000, 1.000000000000000000, -0.000000000000000000 ) ) ;
#11988 = DIRECTION ( 'NONE',  ( 0.000000000000000000, -0.000000000000000000, 1.000000000000000000 ) ) ;
#11989 = CARTESIAN_POINT ( 'NONE',  ( -192.1704923257120754, 141.1970532186197431, 2.500000000000000000 ) ) ;
#11990 = CARTESIAN_POINT ( 'NONE',  ( -64.00000000000002842, 11.87216911405866959, 26.40245448993442068 ) ) ;
#11991 = CARTESIAN_POINT ( 'NONE',  ( -110.0000000000000426, 56.53993994372675047, 13.00000000000000178 ) ) ;
#11992 = ORIENTED_EDGE ( 'NONE', *, *, #7642, .F. ) ;
#11993 = EDGE_LOOP ( 'NONE', ( #10150, #12708, #5625, #12917 ) ) ;
#11994 = DIRECTION ( 'NONE',  ( 0.000000000000000000, 0.000000000000000000, -1.000000000000000000 ) ) ;
#11995 = DIRECTION ( 'NONE',  ( 0.000000000000000000, -1.000000000000000000, 0.000000000000000000 ) ) ;
#11996 = FACE_BOUND ( 'NONE', #1863, .T. ) ;
#11997 = SURFACE_SIDE_STYLE ('',( #6083 ) ) ;
#11998 = DIRECTION ( 'NONE',  ( -0.000000000000000000, -0.000000000000000000, -1.000000000000000000 ) ) ;
#11999 = DIRECTION ( 'NONE',  ( -1.000000000000000000, 0.000000000000000000, 0.000000000000000000 ) ) ;
#12000 = CARTESIAN_POINT ( 'NONE',  ( -214.8715905313398480, 153.8675021612092451, 2.500000000000000000 ) ) ;
#12001 = CIRCLE ( 'NONE', #1384, 1.000000000000000888 ) ;
#12002 = ADVANCED_FACE ( 'NONE', ( #11323 ), #14706, .T. ) ;
#12003 = AXIS2_PLACEMENT_3D ( 'NONE', #7308, #8495, #13277 ) ;
#12004 = ORIENTED_EDGE ( 'NONE', *, *, #3532, .F. ) ;
#12005 = VERTEX_POINT ( 'NONE', #3749 ) ;
#12006 = CARTESIAN_POINT ( 'NONE',  ( 201.3139613293953971, 49.56665511821758230, -6.809528532989353344 ) ) ;
#12007 =( LENGTH_UNIT ( ) NAMED_UNIT ( * ) SI_UNIT ( .MILLI., .METRE. ) );
#12008 = ORIENTED_EDGE ( 'NONE', *, *, #9467, .F. ) ;
#12009 = CARTESIAN_POINT ( 'NONE',  ( -222.6685243335228677, 148.2935983871826977, 9.839440528619144644 ) ) ;
#12010 = ORIENTED_EDGE ( 'NONE', *, *, #14429, .T. ) ;
#12011 = EDGE_LOOP ( 'NONE', ( #8400, #2847, #8922, #10655 ) ) ;
#12012 = LINE ( 'NONE', #12082, #6021 ) ;
#12013 = LINE ( 'NONE', #1180, #2307 ) ;
#12014 = VERTEX_POINT ( 'NONE', #8577 ) ;
#12015 = CARTESIAN_POINT ( 'NONE',  ( 190.0000000000000568, 15.10952649420676863, 9.557440204760682789 ) ) ;
#12016 = EDGE_CURVE ( 'NONE', #4972, #4326, #11018, .T. ) ;
#12017 = DIRECTION ( 'NONE',  ( 3.965082230804130220E-16, 1.486905836551548832E-16, -1.000000000000000000 ) ) ;
#12018 = ORIENTED_EDGE ( 'NONE', *, *, #7513, .F. ) ;
#12019 = VERTEX_POINT ( 'NONE', #168 ) ;
#12020 = CARTESIAN_POINT ( 'NONE',  ( 17.41029453487719181, 40.04259805664093363, 5.000000000000000000 ) ) ;
#12021 = CARTESIAN_POINT ( 'NONE',  ( 64.00000000000005684, 56.53993994372675047, 13.30000000000070948 ) ) ;
#12022 = CARTESIAN_POINT ( 'NONE',  ( -152.4086188282879277, 107.2728346664360402, -4.548387523817075895 ) ) ;
#12023 = ORIENTED_EDGE ( 'NONE', *, *, #7417, .T. ) ;
#12024 = VERTEX_POINT ( 'NONE', #3834 ) ;
#12025 = CARTESIAN_POINT ( 'NONE',  ( -219.4290858278833980, 154.0975609761335932, -2.973479603620232226 ) ) ;
#12026 = CARTESIAN_POINT ( 'NONE',  ( 209.6291075214908801, 33.76515323716659367, -3.385148507280513197 ) ) ;
#12027 = EDGE_LOOP ( 'NONE', ( #10132, #4107, #4728, #4846, #3795, #11005 ) ) ;
#12028 = EDGE_CURVE ( 'NONE', #85, #14199, #8653, .T. ) ;
#12029 = ADVANCED_FACE ( 'NONE', ( #14070, #15244 ), #13924, .T. ) ;
#12030 = CARTESIAN_POINT ( 'NONE',  ( -144.0627431139473345, 95.36268816863731956, 0.000000000000000000 ) ) ;
#12031 = FACE_OUTER_BOUND ( 'NONE', #15535, .T. ) ;
#12032 = ADVANCED_FACE ( 'NONE', ( #6602 ), #8017, .F. ) ;
#12033 = DIRECTION ( 'NONE',  ( 0.000000000000000000, 0.000000000000000000, 1.000000000000000000 ) ) ;
#12034 = ORIENTED_EDGE ( 'NONE', *, *, #1251, .T. ) ;
#12035 = CARTESIAN_POINT ( 'NONE',  ( 205.4339596421060889, 33.86846485884471747, -4.932823326473320336 ) ) ;
#12036 = ORIENTED_EDGE ( 'NONE', *, *, #12857, .T. ) ;
#12037 = FACE_OUTER_BOUND ( 'NONE', #9689, .T. ) ;
#12038 = CARTESIAN_POINT ( 'NONE',  ( -76.50000000000001421, 15.03993994372673981, -2.075184203610571210 ) ) ;
#12039 = CARTESIAN_POINT ( 'NONE',  ( -181.0973828845548610, 120.1829782941312743, 7.859965607560862821 ) ) ;
#12040 = DIRECTION ( 'NONE',  ( -3.965082230804130220E-16, -4.956352788505162775E-17, 1.000000000000000000 ) ) ;
#12041 = EDGE_LOOP ( 'NONE', ( #9513, #14227, #4590, #7520 ) ) ;
#12042 = CARTESIAN_POINT ( 'NONE',  ( -210.8662606591548752, 142.3010704693858486, 10.16010209732750624 ) ) ;
#12043 = CARTESIAN_POINT ( 'NONE',  ( 194.7957337413261030, 33.86335648926068842, -5.558215102112974648 ) ) ;
#12044 = EDGE_CURVE ( 'NONE', #9645, #2958, #2141, .T. ) ;
#12045 = ORIENTED_EDGE ( 'NONE', *, *, #9245, .T. ) ;
#12046 = ORIENTED_EDGE ( 'NONE', *, *, #7108, .F. ) ;
#12047 = CARTESIAN_POINT ( 'NONE',  ( 191.8042410000843745, 59.95507574834591225, 5.000000000000000000 ) ) ;
#12048 = CARTESIAN_POINT ( 'NONE',  ( -155.6477983077465410, 110.1970436846185066, 0.000000000000000000 ) ) ;
#12049 = VECTOR ( 'NONE', #11431, 1000.000000000000000 ) ;
#12050 = CARTESIAN_POINT ( 'NONE',  ( -64.00000000000002842, 15.03993994372673804, 38.07518420361041933 ) ) ;
#12051 = CARTESIAN_POINT ( 'NONE',  ( -139.1458939983161827, 103.0129948961282054, 2.431557144026069928 ) ) ;
#12052 = FACE_OUTER_BOUND ( 'NONE', #1274, .T. ) ;
#12053 = CARTESIAN_POINT ( 'NONE',  ( -223.0788147039891953, 143.0998217501368401, 6.615244852604288184 ) ) ;
#12054 = FACE_OUTER_BOUND ( 'NONE', #382, .T. ) ;
#12055 = DIRECTION ( 'NONE',  ( 0.000000000000000000, -1.734723475976808672E-15, 1.000000000000000000 ) ) ;
#12056 = VECTOR ( 'NONE', #3331, 1000.000000000000000 ) ;
#12057 = ADVANCED_FACE ( 'NONE', ( #1916 ), #10223, .T. ) ;
#12058 = DIRECTION ( 'NONE',  ( 1.000000000000000000, 0.000000000000000000, 0.000000000000000000 ) ) ;
#12059 = CARTESIAN_POINT ( 'NONE',  ( 114.0000000000000426, 17.53993994372673981, 8.693413025030312018E-16 ) ) ;
#12060 = VERTEX_POINT ( 'NONE', #1008 ) ;
#12061 = VERTEX_POINT ( 'NONE', #8104 ) ;
#12062 = AXIS2_PLACEMENT_3D ( 'NONE', #7807, #421, #14956 ) ;
#12063 = EDGE_CURVE ( 'NONE', #9626, #10985, #7964, .T. ) ;
#12064 = ORIENTED_EDGE ( 'NONE', *, *, #791, .F. ) ;
#12065 = DIRECTION ( 'NONE',  ( -0.000000000000000000, -0.000000000000000000, -1.000000000000000000 ) ) ;
#12066 = CARTESIAN_POINT ( 'NONE',  ( 184.0000000000000568, 19.53993994372673626, 48.99999999999997158 ) ) ;
#12067 = CARTESIAN_POINT ( 'NONE',  ( 177.5000000000000853, -181.3058001507315566, -51.45141194869119516 ) ) ;
#12068 = CYLINDRICAL_SURFACE ( 'NONE', #3120, 1.499999999999997780 ) ;
#12069 = CARTESIAN_POINT ( 'NONE',  ( 0.000000000000000000, 0.000000000000000000, 5.000000000000000000 ) ) ;
#12070 = DIRECTION ( 'NONE',  ( -0.000000000000000000, 1.000000000000000000, -0.000000000000000000 ) ) ;
#12071 = CYLINDRICAL_SURFACE ( 'NONE', #185, 0.5000000000000004441 ) ;
#12072 = EDGE_LOOP ( 'NONE', ( #5814, #2594, #4785, #2651 ) ) ;
#12073 = AXIS2_PLACEMENT_3D ( 'NONE', #10536, #15332, #894 ) ;
#12074 = TOROIDAL_SURFACE ( 'NONE', #15333, 1.000000000000000000, 0.5000000000000000000 ) ;
#12075 = ORIENTED_EDGE ( 'NONE', *, *, #8939, .F. ) ;
#12076 = CARTESIAN_POINT ( 'NONE',  ( 207.0793923465612352, 46.18607573428356972, -5.755770042397863051 ) ) ;
#12077 = VERTEX_POINT ( 'NONE', #9123 ) ;
#12078 = AXIS2_PLACEMENT_3D ( 'NONE', #2239, #1284, #13 ) ;
#12079 = CARTESIAN_POINT ( 'NONE',  ( -223.1412712182228972, 147.4465981345315981, 7.416791562717193642 ) ) ;
#12080 = EDGE_LOOP ( 'NONE', ( #13155, #10171, #11289, #4328 ) ) ;
#12081 = VERTEX_POINT ( 'NONE', #5563 ) ;
#12082 = CARTESIAN_POINT ( 'NONE',  ( 177.5000000000000853, -179.2362136002515740, 53.26098611522623827 ) ) ;
#12083 = FACE_OUTER_BOUND ( 'NONE', #15384, .T. ) ;
#12084 = ORIENTED_EDGE ( 'NONE', *, *, #8498, .F. ) ;
#12085 = DIRECTION ( 'NONE',  ( 1.000000000000000000, 0.000000000000000000, 0.000000000000000000 ) ) ;
#12086 = LINE ( 'NONE', #1264, #480 ) ;
#12087 = EDGE_CURVE ( 'NONE', #6953, #3135, #12652, .T. ) ;
#12088 = AXIS2_PLACEMENT_3D ( 'NONE', #12413, #558, #396 ) ;
#12089 = DIRECTION ( 'NONE',  ( 1.000000000000000000, 0.000000000000000000, 0.000000000000000000 ) ) ;
#12090 = AXIS2_PLACEMENT_3D ( 'NONE', #6122, #7395, #1609 ) ;
#12091 = EDGE_CURVE ( 'NONE', #12821, #2912, #6189, .T. ) ;
#12092 = VERTEX_POINT ( 'NONE', #646 ) ;
#12093 =( REPRESENTATION_RELATIONSHIP ('NONE','NONE', #3298, #556 ) REPRESENTATION_RELATIONSHIP_WITH_TRANSFORMATION ( #14990 )SHAPE_REPRESENTATION_RELATIONSHIP( ) );
#12094 = ORIENTED_EDGE ( 'NONE', *, *, #15080, .F. ) ;
#12095 = CARTESIAN_POINT ( 'NONE',  ( 177.5000000000000853, -178.8058001507315566, 65.31842631998698323 ) ) ;
#12096 = EDGE_CURVE ( 'NONE', #592, #3561, #13762, .T. ) ;
#12097 = DIRECTION ( 'NONE',  ( -0.4873681696970831312, -0.8731965799097676229, 0.000000000000000000 ) ) ;
#12098 = CIRCLE ( 'NONE', #5294, 1.700000000000000178 ) ;
#12099 = VERTEX_POINT ( 'NONE', #2075 ) ;
#12100 = ORIENTED_EDGE ( 'NONE', *, *, #1378, .F. ) ;
#12101 = CARTESIAN_POINT ( 'NONE',  ( -173.2995934586704152, 128.4510609142004114, -2.983067475588502937 ) ) ;
#12102 = CARTESIAN_POINT ( 'NONE',  ( 208.8071490909987347, 39.71769555335276891, -3.129532392942456553 ) ) ;
#12103 = ORIENTED_EDGE ( 'NONE', *, *, #9274, .F. ) ;
#12104 = PLANE ( 'NONE',  #9829 ) ;
#12105 = DIRECTION ( 'NONE',  ( 1.077120774387149835E-15, 0.9902680687415711391, -0.1391731009600592484 ) ) ;
#12106 = DIRECTION ( 'NONE',  ( 0.000000000000000000, -0.1391731009600592484, -0.9902680687415712502 ) ) ;
#12107 = AXIS2_PLACEMENT_3D ( 'NONE', #7136, #11940, #5932 ) ;
#12108 = ORIENTED_EDGE ( 'NONE', *, *, #14922, .F. ) ;
#12109 = CIRCLE ( 'NONE', #11615, 4.499999999999950262 ) ;
#12110 = AXIS2_PLACEMENT_3D ( 'NONE', #2819, #7641, #12433 ) ;
#12111 =( NAMED_UNIT ( * ) PLANE_ANGLE_UNIT ( ) SI_UNIT ( $, .RADIAN. ) );
#12112 = CARTESIAN_POINT ( 'NONE',  ( 198.8340532681795594, 32.16525826020106393, -3.739820046187162905 ) ) ;
#12113 = ORIENTED_EDGE ( 'NONE', *, *, #5928, .F. ) ;
#12114 = DIRECTION ( 'NONE',  ( 0.000000000000000000, 0.000000000000000000, -1.000000000000000000 ) ) ;
#12115 = CARTESIAN_POINT ( 'NONE',  ( 172.5293059057019889, 61.25683321636181233, 7.600000000000002309 ) ) ;
#12116 = CARTESIAN_POINT ( 'NONE',  ( -173.0737465816261818, 117.4314230949052558, 7.694953281110847421 ) ) ;
#12119 = ADVANCED_FACE ( 'NONE', ( #6907 ), #1377, .F. ) ;
#12118 = EDGE_CURVE ( 'NONE', #5947, #10243, #8222, .T. ) ;
#12117 = CARTESIAN_POINT ( 'NONE',  ( 178.0000000000000853, -178.8058001507315566, -18.19066787724516843 ) ) ;
#12120 = ORIENTED_EDGE ( 'NONE', *, *, #14792, .F. ) ;
#12121 = CARTESIAN_POINT ( 'NONE',  ( -170.7405378081422214, 121.6209906574826931, 10.02899269843361374 ) ) ;
#12122 = DIRECTION ( 'NONE',  ( -0.000000000000000000, 1.000000000000000000, -0.000000000000000000 ) ) ;
#12123 = VERTEX_POINT ( 'NONE', #1765 ) ;
#12124 = ORIENTED_EDGE ( 'NONE', *, *, #13336, .T. ) ;
#12125 = AXIS2_PLACEMENT_3D ( 'NONE', #10016, #14797, #8452 ) ;
#12126 = EDGE_CURVE ( 'NONE', #13704, #3979, #14940, .T. ) ;
#12127 = CARTESIAN_POINT ( 'NONE',  ( -174.2824251065520968, 115.9783496305641535, 2.177446462082195389 ) ) ;
#12128 = DIRECTION ( 'NONE',  ( 1.000000000000000000, 0.000000000000000000, 0.000000000000000000 ) ) ;
#12129 = VECTOR ( 'NONE', #5308, 1000.000000000000000 ) ;
#12130 = CARTESIAN_POINT ( 'NONE',  ( 0.08285530295199074191, 1.570896314769977931, 8.000000000000007105 ) ) ;
#12131 = LINE ( 'NONE', #15511, #1913 ) ;
#12132 = CARTESIAN_POINT ( 'NONE',  ( -225.4439234422023617, 143.3210352198185547, -0.3244446825575932891 ) ) ;
#12133 = DIRECTION ( 'NONE',  ( -1.000000000000000000, 0.000000000000000000, 0.000000000000000000 ) ) ;
#12134 = AXIS2_PLACEMENT_3D ( 'NONE', #3544, #8378, #13160 ) ;
#12135 = CARTESIAN_POINT ( 'NONE',  ( -157.6232119703703631, 109.9408540656516067, 9.325089004845752427 ) ) ;
#12136 = EDGE_CURVE ( 'NONE', #11949, #15030, #15017, .T. ) ;
#12137 = DIRECTION ( 'NONE',  ( -0.000000000000000000, -0.000000000000000000, 1.000000000000000000 ) ) ;
#12138 = VECTOR ( 'NONE', #7242, 1000.000000000000000 ) ;
#12139 = FACE_OUTER_BOUND ( 'NONE', #15187, .T. ) ;
#12140 = VERTEX_POINT ( 'NONE', #7783 ) ;
#12141 = ORIENTED_EDGE ( 'NONE', *, *, #3635, .F. ) ;
#12142 = LINE ( 'NONE', #6080, #10285 ) ;
#12143 = DIRECTION ( 'NONE',  ( 0.000000000000000000, 4.956352788505162775E-17, -1.000000000000000000 ) ) ;
#12144 = FACE_OUTER_BOUND ( 'NONE', #13103, .T. ) ;
#12145 = EDGE_CURVE ( 'NONE', #11235, #11925, #13229, .T. ) ;
#12146 = CARTESIAN_POINT ( 'NONE',  ( 190.0000000000000568, -178.8058001507315566, 52.19066787724494816 ) ) ;
#12147 = DIRECTION ( 'NONE',  ( 0.000000000000000000, -1.000000000000000000, 0.000000000000000000 ) ) ;
#12148 = DIRECTION ( 'NONE',  ( -0.000000000000000000, 1.000000000000000000, -0.000000000000000000 ) ) ;
#12149 = CARTESIAN_POINT ( 'NONE',  ( -192.1748460459477030, 141.1892528453990110, 3.478855109513427468 ) ) ;
#12150 = CIRCLE ( 'NONE', #13406, 1.000000000000000888 ) ;
#12151 = ORIENTED_EDGE ( 'NONE', *, *, #11823, .F. ) ;
#12152 = ADVANCED_FACE ( 'NONE', ( #6751 ), #10456, .F. ) ;
#12153 = ORIENTED_EDGE ( 'NONE', *, *, #15322, .F. ) ;
#12154 = CYLINDRICAL_SURFACE ( 'NONE', #15156, 1.499999999999994449 ) ;
#12155 = EDGE_LOOP ( 'NONE', ( #7734, #15612 ) ) ;
#12156 = VECTOR ( 'NONE', #402, 1000.000000000000000 ) ;
#12157 = CARTESIAN_POINT ( 'NONE',  ( -223.4491651843841282, 142.3567805253620691, 4.912650739265252753 ) ) ;
#12158 = VERTEX_POINT ( 'NONE', #6682 ) ;
#12159 = DIRECTION ( 'NONE',  ( 0.000000000000000000, 0.000000000000000000, -1.000000000000000000 ) ) ;
#12160 = AXIS2_PLACEMENT_3D ( 'NONE', #10345, #9171, #13971 ) ;
#12161 = CARTESIAN_POINT ( 'NONE',  ( 207.3258607540788319, 31.40438376407220389, -4.939321231805051227 ) ) ;
#12162 = ORIENTED_EDGE ( 'NONE', *, *, #11075, .T. ) ;
#12163 = CARTESIAN_POINT ( 'NONE',  ( 190.0000000000000568, 14.90076684276668040, -2.084916134869001958 ) ) ;
#12164 = DIRECTION ( 'NONE',  ( 1.000000000000000000, -0.000000000000000000, -0.000000000000000000 ) ) ;
#12165 = CYLINDRICAL_SURFACE ( 'NONE', #1069, 3.500000000000003109 ) ;
#12166 = ORIENTED_EDGE ( 'NONE', *, *, #7868, .T. ) ;
#12167 = CIRCLE ( 'NONE', #10923, 1.499999999999997780 ) ;
#12168 = ORIENTED_EDGE ( 'NONE', *, *, #4052, .F. ) ;
#12169 = CARTESIAN_POINT ( 'NONE',  ( 151.6469155423420716, 8.238904255104483099, -6.725526318947268045 ) ) ;
#12170 = CARTESIAN_POINT ( 'NONE',  ( 190.5000000000000853, -179.8058001507315566, 84.88378295107887084 ) ) ;
#12171 = ORIENTED_EDGE ( 'NONE', *, *, #9853, .T. ) ;
#12172 = AXIS2_PLACEMENT_3D ( 'NONE', #538, #2854, #7756 ) ;
#12173 = CARTESIAN_POINT ( 'NONE',  ( -63.50000000000002842, -179.2362136002515740, 53.26098611522623827 ) ) ;
#12174 = CARTESIAN_POINT ( 'NONE',  ( -76.00000000000004263, -178.8753867012115961, 64.82329228561619061 ) ) ;
#12175 = ORIENTED_EDGE ( 'NONE', *, *, #15293, .T. ) ;
#12176 = ORIENTED_EDGE ( 'NONE', *, *, #822, .T. ) ;
#12177 = CARTESIAN_POINT ( 'NONE',  ( -185.3517468524019591, 137.0386009272039871, -0.4547266291960738172 ) ) ;
#12178 = CARTESIAN_POINT ( 'NONE',  ( -223.6145774380523505, 142.0129443944823606, 2.393984899497048513 ) ) ;
#12179 = ORIENTED_EDGE ( 'NONE', *, *, #7021, .F. ) ;
#12180 = AXIS2_PLACEMENT_3D ( 'NONE', #14179, #4794, #15356 ) ;
#12181 = CARTESIAN_POINT ( 'NONE',  ( 15.71029453487719074, 40.04259805664093363, 10.00000000000000178 ) ) ;
#12182 = DIRECTION ( 'NONE',  ( 0.4873681696970824651, 0.8731965799097680669, 0.000000000000000000 ) ) ;
#12183 = CARTESIAN_POINT ( 'NONE',  ( -63.50000000000002842, 16.03993994372673981, 25.38206912977649665 ) ) ;
#12184 = EDGE_CURVE ( 'NONE', #1565, #2746, #11557, .T. ) ;
#12185 = VERTEX_POINT ( 'NONE', #9425 ) ;
#12186 = CARTESIAN_POINT ( 'NONE',  ( 188.3378656401271201, 39.26133998289535043, -1.370343197488200548 ) ) ;
#12187 = VERTEX_POINT ( 'NONE', #13114 ) ;
#12188 = DIRECTION ( 'NONE',  ( 0.000000000000000000, 0.000000000000000000, -1.000000000000000000 ) ) ;
#12189 = CARTESIAN_POINT ( 'NONE',  ( -218.3491273834486890, 151.9915237902018248, -3.871359521417834237 ) ) ;
#12190 = CARTESIAN_POINT ( 'NONE',  ( -191.3370974917540366, 126.0439545877573266, -0.4555467707853441128 ) ) ;
#12191 = FACE_OUTER_BOUND ( 'NONE', #12011, .T. ) ;
#12192 = ORIENTED_EDGE ( 'NONE', *, *, #6928, .F. ) ;
#12193 = CARTESIAN_POINT ( 'NONE',  ( -178.4568510201948186, 124.9139056227158733, 10.12588066961104261 ) ) ;
#12194 = CARTESIAN_POINT ( 'NONE',  ( 193.1249951165660548, 46.22013307728793308, -3.310989833511668756 ) ) ;
#12195 = VECTOR ( 'NONE', #14485, 1000.000000000000000 ) ;
#12196 = ORIENTED_EDGE ( 'NONE', *, *, #3880, .T. ) ;
#12197 = VERTEX_POINT ( 'NONE', #3494 ) ;
#12198 = DIRECTION ( 'NONE',  ( 3.965082230804130220E-16, -1.486905836551548832E-16, 1.000000000000000000 ) ) ;
#12199 = ADVANCED_FACE ( 'NONE', ( #882 ), #8411, .T. ) ;
#12200 = DIRECTION ( 'NONE',  ( 0.000000000000000000, 0.000000000000000000, 1.000000000000000000 ) ) ;
#12201 = CARTESIAN_POINT ( 'NONE',  ( 175.9483885134608272, -178.8058001507315566, -17.19066787724516843 ) ) ;
#12202 = FACE_OUTER_BOUND ( 'NONE', #12832, .T. ) ;
#12203 = VECTOR ( 'NONE', #14834, 1000.000000000000000 ) ;
#12204 = EDGE_CURVE ( 'NONE', #11543, #6413, #7064, .T. ) ;
#12205 = EDGE_CURVE ( 'NONE', #8310, #14585, #4843, .T. ) ;
#12206 = VECTOR ( 'NONE', #7914, 1000.000000000000000 ) ;
#12207 = DIRECTION ( 'NONE',  ( -0.000000000000000000, -0.000000000000000000, 1.000000000000000000 ) ) ;
#12208 = EDGE_CURVE ( 'NONE', #1178, #14048, #4414, .T. ) ;
#12209 = ADVANCED_FACE ( 'NONE', ( #5785 ), #15479, .F. ) ;
#12210 = DIRECTION ( 'NONE',  ( -0.000000000000000000, 1.000000000000000000, -0.000000000000000000 ) ) ;
#12211 = PLANE ( 'NONE',  #12805 ) ;
#12212 = CARTESIAN_POINT ( 'NONE',  ( -155.6477983077465410, 110.1970436846185066, 84.88378295107887084 ) ) ;
#12213 = ORIENTED_EDGE ( 'NONE', *, *, #3994, .F. ) ;
#12214 = CARTESIAN_POINT ( 'NONE',  ( -5.196152422706630247, -9.000000000000005329, 0.000000000000000000 ) ) ;
#12215 = CIRCLE ( 'NONE', #7695, 1.700000000000000178 ) ;
#12216 = EDGE_LOOP ( 'NONE', ( #3281, #13684, #3330, #7792 ) ) ;
#12217 = DIRECTION ( 'NONE',  ( 0.000000000000000000, 0.000000000000000000, -1.000000000000000000 ) ) ;
#12218 = CARTESIAN_POINT ( 'NONE',  ( -64.00000000000002842, 15.53993994372673804, 37.49999999999991473 ) ) ;
#12219 = CARTESIAN_POINT ( 'NONE',  ( 190.5000000000000568, 15.03993994372673981, 10.05257423913146475 ) ) ;
#12220 = CARTESIAN_POINT ( 'NONE',  ( -1.302788261070087384E-15, 2.652070323102390770, -0.9064794551410521040 ) ) ;
#12221 = FACE_OUTER_BOUND ( 'NONE', #13331, .T. ) ;
#12222 = CARTESIAN_POINT ( 'NONE',  ( 0.09566599640798266468, -1.847441354476797359, -2.300137710042325256 ) ) ;
#12223 = CARTESIAN_POINT ( 'NONE',  ( -76.00000000000004263, 15.10952649420676686, 25.44255979523916977 ) ) ;
#12224 = EDGE_CURVE ( 'NONE', #14758, #7532, #3649, .T. ) ;
#12225 = EDGE_CURVE ( 'NONE', #944, #12081, #9979, .T. ) ;
#12226 = EDGE_CURVE ( 'NONE', #13651, #4381, #3160, .T. ) ;
#12227 = ORIENTED_EDGE ( 'NONE', *, *, #455, .T. ) ;
#12228 = VECTOR ( 'NONE', #2409, 1000.000000000000000 ) ;
#12229 = CARTESIAN_POINT ( 'NONE',  ( -224.6033116245361043, 144.8271232449910713, 2.544233000457407634 ) ) ;
#12230 = ORIENTED_EDGE ( 'NONE', *, *, #12557, .F. ) ;
#12231 = CARTESIAN_POINT ( 'NONE',  ( -224.9759671128498439, 144.1594524405806510, 6.941577500106505205 ) ) ;
#12232 = ORIENTED_EDGE ( 'NONE', *, *, #4164, .F. ) ;
#12233 = CARTESIAN_POINT ( 'NONE',  ( -171.4210576570572471, 121.1049385752565541, -5.124804266949916531 ) ) ;
#12234 = CARTESIAN_POINT ( 'NONE',  ( 188.3564733894159815, 42.55163899863504184, -6.069020498571065403 ) ) ;
#12235 = EDGE_CURVE ( 'NONE', #10091, #8109, #9351, .T. ) ;
#12236 = VERTEX_POINT ( 'NONE', #5943 ) ;
#12237 = LINE ( 'NONE', #14679, #2089 ) ;
#12238 = DIRECTION ( 'NONE',  ( 1.000000000000000000, 0.000000000000000000, 0.000000000000000000 ) ) ;
#12239 = AXIS2_PLACEMENT_3D ( 'NONE', #7460, #7390, #6118 ) ;
#12240 = CARTESIAN_POINT ( 'NONE',  ( 114.0000000000000568, 56.53993994372675047, 16.70000000000034746 ) ) ;
#12241 = EDGE_LOOP ( 'NONE', ( #14435, #11507, #4962, #10513 ) ) ;
#12242 = CARTESIAN_POINT ( 'NONE',  ( -70.00000000000000000, 21.53993994372675758, 47.49999999999997868 ) ) ;
#12243 = AXIS2_PLACEMENT_3D ( 'NONE', #2053, #6891, #15301 ) ;
#12244 = ORIENTED_EDGE ( 'NONE', *, *, #4319, .T. ) ;
#12245 = LINE ( 'NONE', #8780, #14355 ) ;
#12246 = ORIENTED_EDGE ( 'NONE', *, *, #2352, .F. ) ;
#12247 = LINE ( 'NONE', #12173, #7220 ) ;
#12248 = ADVANCED_FACE ( 'NONE', ( #13029 ), #7226, .F. ) ;
#12249 = CARTESIAN_POINT ( 'NONE',  ( 2.000000000000000000, 0.000000000000000000, 0.000000000000000000 ) ) ;
#12250 = ORIENTED_EDGE ( 'NONE', *, *, #445, .F. ) ;
#12251 = ORIENTED_EDGE ( 'NONE', *, *, #2572, .T. ) ;
#12252 = CARTESIAN_POINT ( 'NONE',  ( -211.2943419521749888, 151.8811774793218490, 1.515441477536285220 ) ) ;
#12253 = CARTESIAN_POINT ( 'NONE',  ( 201.2541767070109984, 32.14103196098812987, -5.186035738131804962 ) ) ;
#12254 = EDGE_LOOP ( 'NONE', ( #11501, #8490, #10627, #13525, #10109, #9096, #215, #79, #10992, #13868, #4014, #7892, #4650, #11014 ) ) ;
#12255 = FACE_OUTER_BOUND ( 'NONE', #1391, .T. ) ;
#12256 = DIRECTION ( 'NONE',  ( 1.000000000000000000, 0.000000000000000000, 0.000000000000000000 ) ) ;
#12257 = DIRECTION ( 'NONE',  ( -0.000000000000000000, 1.000000000000000000, -0.000000000000000000 ) ) ;
#12258 = VECTOR ( 'NONE', #10718, 1000.000000000000000 ) ;
#12259 = FACE_BOUND ( 'NONE', #9883, .T. ) ;
#12260 = EDGE_CURVE ( 'NONE', #8201, #5020, #2152, .T. ) ;
#12261 = CARTESIAN_POINT ( 'NONE',  ( 205.4727397017886119, 47.82775141623291404, -2.488642475836487566 ) ) ;
#12262 = ORIENTED_EDGE ( 'NONE', *, *, #225, .F. ) ;
#12263 = CARTESIAN_POINT ( 'NONE',  ( 185.1062858801516882, 55.86394065090267702, 18.00000000000000355 ) ) ;
#12264 = CARTESIAN_POINT ( 'NONE',  ( -218.5464654778641034, 151.6367060758224454, -4.121322150339921109 ) ) ;
#12265 = CARTESIAN_POINT ( 'NONE',  ( -216.9311889273521672, 150.1826874172201656, -4.640918829492440167 ) ) ;
#12266 = LINE ( 'NONE', #6284, #9555 ) ;
#12267 = ORIENTED_EDGE ( 'NONE', *, *, #8427, .T. ) ;
#12268 = EDGE_CURVE ( 'NONE', #14171, #8310, #14296, .T. ) ;
#12269 = CARTESIAN_POINT ( 'NONE',  ( -175.8847466161772957, 123.8162673009714752, 10.09358467921856573 ) ) ;
#12270 = CARTESIAN_POINT ( 'NONE',  ( 207.1663125311009992, 46.09156421935289671, -5.616260741029326375 ) ) ;
#12271 = ORIENTED_EDGE ( 'NONE', *, *, #3338, .F. ) ;
#12272 = EDGE_LOOP ( 'NONE', ( #10161, #9047, #9044, #3964, #277 ) ) ;
#12273 = CARTESIAN_POINT ( 'NONE',  ( -63.50000000000002842, -178.8058001507315566, 52.19066787724494816 ) ) ;
#12274 = CARTESIAN_POINT ( 'NONE',  ( 170.6931741512129577, -3.595212766542494887, -13.46247879130521952 ) ) ;
#12275 = ADVANCED_FACE ( 'NONE', ( #13188 ), #4755, .F. ) ;
#12276 = CARTESIAN_POINT ( 'NONE',  ( 190.5000000000000568, 17.53993994372673981, -17.50000000000002487 ) ) ;
#12277 = CARTESIAN_POINT ( 'NONE',  ( 215.1062858801516882, 25.86394065090268057, 18.00000000000000355 ) ) ;
#12278 = CARTESIAN_POINT ( 'NONE',  ( -64.00000000000002842, -179.8058001507315566, 52.49999999999997868 ) ) ;
#12279 = CARTESIAN_POINT ( 'NONE',  ( -185.3757041553864156, 136.9956776582455973, 5.434754235172603920 ) ) ;
#12280 = CARTESIAN_POINT ( 'NONE',  ( 200.1062858801516597, 40.86394065090267702, 10.00000000000000000 ) ) ;
#12281 = DIRECTION ( 'NONE',  ( 0.000000000000000000, 0.000000000000000000, -1.000000000000000000 ) ) ;
#12282 = ORIENTED_EDGE ( 'NONE', *, *, #7340, .T. ) ;
#12283 = DIRECTION ( 'NONE',  ( -0.000000000000000000, -1.000000000000000000, -0.000000000000000000 ) ) ;
#12284 = EDGE_CURVE ( 'NONE', #5947, #12618, #14150, .T. ) ;
#12285 = AXIS2_PLACEMENT_3D ( 'NONE', #7911, #3083, #4409 ) ;
#12286 = ORIENTED_EDGE ( 'NONE', *, *, #13550, .T. ) ;
#12287 = DIRECTION ( 'NONE',  ( -0.000000000000000000, -0.9902680687415712502, -0.1391731009600584990 ) ) ;
#12288 = CARTESIAN_POINT ( 'NONE',  ( 6.800000000000000711, 0.000000000000000000, 0.000000000000000000 ) ) ;
#12289 = DIRECTION ( 'NONE',  ( -0.2258817899775119320, -0.9741547192086866813, 0.000000000000000000 ) ) ;
#12290 = AXIS2_PLACEMENT_3D ( 'NONE', #14182, #5905, #2270 ) ;
#12291 = CARTESIAN_POINT ( 'NONE',  ( 5.799999999999999822, -9.237604307034018802, 2.775557561562891351E-14 ) ) ;
#12292 = CARTESIAN_POINT ( 'NONE',  ( -70.00000000000000000, 17.53993994372673981, -12.49999999999999467 ) ) ;
#12293 = LINE ( 'NONE', #13714, #9257 ) ;
#12294 = DIRECTION ( 'NONE',  ( 0.000000000000000000, 0.000000000000000000, 1.000000000000000000 ) ) ;
#12295 = CARTESIAN_POINT ( 'NONE',  ( -177.3600541072865155, 132.9204870282739819, 3.478855109513427468 ) ) ;
#12296 = EDGE_LOOP ( 'NONE', ( #2575, #7833, #5004, #9965 ) ) ;
#12297 = VECTOR ( 'NONE', #5594, 1000.000000000000000 ) ;
#12298 = CARTESIAN_POINT ( 'NONE',  ( 114.0000000000000568, 59.53993994372674337, 16.70000000000034746 ) ) ;
#12299 = CONICAL_SURFACE ( 'NONE', #12802, 3.525000000000002132, 0.7853981633974482790 ) ;
#12300 = VECTOR ( 'NONE', #14494, 1000.000000000000000 ) ;
#12301 = CARTESIAN_POINT ( 'NONE',  ( -85.99999999999994316, 64.53993994372673626, 13.30000000000175575 ) ) ;
#12302 = LINE ( 'NONE', #11055, #6361 ) ;
#12303 = EDGE_LOOP ( 'NONE', ( #5024, #10813, #2890, #10229 ) ) ;
#12304 = EDGE_CURVE ( 'NONE', #2049, #14442, #10849, .T. ) ;
#12305 = CARTESIAN_POINT ( 'NONE',  ( -216.7483548245723455, 154.8006932417845860, 3.755670596743044598 ) ) ;
#12307 = EDGE_CURVE ( 'NONE', #1126, #13122, #6987, .T. ) ;
#12306 = EDGE_CURVE ( 'NONE', #4671, #7084, #13490, .T. ) ;
#12308 = VERTEX_POINT ( 'NONE', #9739 ) ;
#12309 = CARTESIAN_POINT ( 'NONE',  ( -34.79899788034579444, 48.72489408690345414, 10.00000000000000178 ) ) ;
#12310 = CARTESIAN_POINT ( 'NONE',  ( 203.1913894652216186, 29.76335179383669782, -8.124653964949581919 ) ) ;
#12311 = VERTEX_POINT ( 'NONE', #7379 ) ;
#12312 = AXIS2_PLACEMENT_3D ( 'NONE', #3785, #8530, #12881 ) ;
#12313 = CARTESIAN_POINT ( 'NONE',  ( 177.5000000000000853, 15.17911304468680100, 9.062306170389884841 ) ) ;
#12314 = DIRECTION ( 'NONE',  ( 0.4999999999999997224, 0.8660254037844387076, 0.000000000000000000 ) ) ;
#12315 = AXIS2_PLACEMENT_3D ( 'NONE', #12905, #9366, #2166 ) ;
#12316 = AXIS2_PLACEMENT_3D ( 'NONE', #6932, #1067, #8354 ) ;
#12317 = FACE_BOUND ( 'NONE', #5790, .T. ) ;
#12318 = ORIENTED_EDGE ( 'NONE', *, *, #915, .T. ) ;
#12319 = DIRECTION ( 'NONE',  ( 0.7580103477576812798, -0.4387477715939339662, -0.4826185922792826100 ) ) ;
#12320 = ORIENTED_EDGE ( 'NONE', *, *, #6344, .T. ) ;
#12321 = FILL_AREA_STYLE_COLOUR ( '', #8337 ) ;
#12322 = CIRCLE ( 'NONE', #5025, 0.5000000000000000000 ) ;
#12323 = CARTESIAN_POINT ( 'NONE',  ( 163.3793289068652541, 15.80605437029534954, -6.370175303308202253 ) ) ;
#12324 = ORIENTED_EDGE ( 'NONE', *, *, #14236, .T. ) ;
#12325 = DIRECTION ( 'NONE',  ( 1.000000000000000000, -2.751328491981765035E-32, 3.965082230804130220E-16 ) ) ;
#12326 = AXIS2_PLACEMENT_3D ( 'NONE', #2810, #7631, #1615 ) ;
#12327 = CARTESIAN_POINT ( 'NONE',  ( -151.1649979179899219, 108.2517653509981841, -4.957866620889593179 ) ) ;
#12328 = ORIENTED_EDGE ( 'NONE', *, *, #11468, .F. ) ;
#12329 = VERTEX_POINT ( 'NONE', #8555 ) ;
#12330 = CARTESIAN_POINT ( 'NONE',  ( -179.9267697467775520, 134.3633106217456543, 2.500000000000000000 ) ) ;
#12331 = CARTESIAN_POINT ( 'NONE',  ( 205.4496313998743915, 47.84832575209421890, -7.060263518810960370 ) ) ;
#12332 = ORIENTED_EDGE ( 'NONE', *, *, #13260, .F. ) ;
#12333 = FACE_OUTER_BOUND ( 'NONE', #5177, .T. ) ;
#12334 = FACE_OUTER_BOUND ( 'NONE', #1086, .T. ) ;
#12335 = AXIS2_PLACEMENT_3D ( 'NONE', #5235, #1600, #11086 ) ;
#12336 = DIRECTION ( 'NONE',  ( 0.000000000000000000, -6.938893903907222067E-15, 1.000000000000000000 ) ) ;
#12337 = AXIS2_PLACEMENT_3D ( 'NONE', #4568, #8147, #5681 ) ;
#12338 = EDGE_CURVE ( 'NONE', #14309, #50, #8479, .T. ) ;
#12339 = DIRECTION ( 'NONE',  ( 0.000000000000000000, 4.956352788505162775E-17, -1.000000000000000000 ) ) ;
#12340 = AXIS2_PLACEMENT_3D ( 'NONE', #981, #15423, #10477 ) ;
#12341 = CARTESIAN_POINT ( 'NONE',  ( 202.9867918041427686, 48.86553571320913392, 0.6621522355815065985 ) ) ;
#12342 = ORIENTED_EDGE ( 'NONE', *, *, #9225, .T. ) ;
#12343 = FACE_BOUND ( 'NONE', #9166, .T. ) ;
#12344 = CARTESIAN_POINT ( 'NONE',  ( -223.2729691302634194, 142.6739754659882919, -0.8558400769978052880 ) ) ;
#12345 = COLOUR_RGB ( '', 0.72549020, 0.75294118, 0.79215686) ;
#12346 = CARTESIAN_POINT ( 'NONE',  ( -204.9433645127610646, 133.1096489332827275, -2.964974570226844186 ) ) ;
#12347 = CIRCLE ( 'NONE', #2009, 1.700000000000000178 ) ;
#12348 = CARTESIAN_POINT ( 'NONE',  ( -76.00000000000001421, 14.97035339324670922, -2.580050169239785696 ) ) ;
#12349 = ORIENTED_EDGE ( 'NONE', *, *, #2387, .F. ) ;
#12350 = CARTESIAN_POINT ( 'NONE',  ( -194.4337897068680547, 127.2572260587109554, 1.515400478619095992 ) ) ;
#12351 = AXIS2_PLACEMENT_3D ( 'NONE', #6748, #3414, #12799 ) ;
#12352 = CARTESIAN_POINT ( 'NONE',  ( 205.3747499027128924, 33.81850075496041796, -3.363818451488727934 ) ) ;
#12353 = ORIENTED_EDGE ( 'NONE', *, *, #1861, .F. ) ;
#12354 = ORIENTED_EDGE ( 'NONE', *, *, #2804, .T. ) ;
#12355 = DIRECTION ( 'NONE',  ( 0.000000000000000000, 0.000000000000000000, 1.000000000000000000 ) ) ;
#12356 = DIRECTION ( 'NONE',  ( 1.000000000000000000, 0.000000000000000000, 0.000000000000000000 ) ) ;
#12357 = VECTOR ( 'NONE', #5863, 1000.000000000000000 ) ;
#12358 = CYLINDRICAL_SURFACE ( 'NONE', #6580, 0.5000000000000004441 ) ;
#12359 = VECTOR ( 'NONE', #1939, 1000.000000000000000 ) ;
#12360 = AXIS2_PLACEMENT_3D ( 'NONE', #8981, #13774, #8817 ) ;
#12361 = EDGE_CURVE ( 'NONE', #3648, #6413, #2787, .T. ) ;
#12362 = PLANE ( 'NONE',  #1852 ) ;
#12363 = DIRECTION ( 'NONE',  ( -0.000000000000000000, 1.000000000000000000, -0.000000000000000000 ) ) ;
#12364 = DIRECTION ( 'NONE',  ( -0.000000000000000000, -8.673617379884035472E-17, 1.000000000000000000 ) ) ;
#12365 = AXIS2_PLACEMENT_3D ( 'NONE', #13893, #9093, #3088 ) ;
#12366 = DIRECTION ( 'NONE',  ( -0.000000000000000000, 1.000000000000000000, 1.156482317317871725E-16 ) ) ;
#12367 = EDGE_LOOP ( 'NONE', ( #3418, #1193, #14441, #7526 ) ) ;
#12369 = VECTOR ( 'NONE', #3995, 1000.000000000000000 ) ;
#12368 = DIRECTION ( 'NONE',  ( -0.000000000000000000, 1.000000000000000000, 0.000000000000000000 ) ) ;
#12370 = ORIENTED_EDGE ( 'NONE', *, *, #11499, .T. ) ;
#12371 = VERTEX_POINT ( 'NONE', #9978 ) ;
#12372 = CARTESIAN_POINT ( 'NONE',  ( -151.6951454547776166, 108.2398202450613098, 9.769994122432189343 ) ) ;
#12373 = CARTESIAN_POINT ( 'NONE',  ( 190.5000000000000853, -179.8058001507315566, 65.31842631998698323 ) ) ;
#12374 =( NAMED_UNIT ( * ) SI_UNIT ( $, .STERADIAN. ) SOLID_ANGLE_UNIT ( ) );
#12375 = DIRECTION ( 'NONE',  ( -0.000000000000000000, -1.000000000000000000, -0.000000000000000000 ) ) ;
#12376 = DIRECTION ( 'NONE',  ( -3.965082230804130220E-16, -4.956352788505162775E-17, 1.000000000000000000 ) ) ;
#12377 = DIRECTION ( 'NONE',  ( -0.000000000000000000, -0.000000000000000000, 1.000000000000000000 ) ) ;
#12378 = CARTESIAN_POINT ( 'NONE',  ( -188.0905678060899220, 138.5068454852687125, 5.434754235172603920 ) ) ;
#12379 = ORIENTED_EDGE ( 'NONE', *, *, #6005, .T. ) ;
#12380 = CIRCLE ( 'NONE', #4828, 1.700000000000000178 ) ;
#12381 = EDGE_CURVE ( 'NONE', #13013, #15505, #13581, .T. ) ;
#12382 = CYLINDRICAL_SURFACE ( 'NONE', #7921, 1.499999999999994449 ) ;
#12383 = CIRCLE ( 'NONE', #1543, 0.5000000000000004441 ) ;
#12384 = DIRECTION ( 'NONE',  ( 0.000000000000000000, 0.4999999999999996669, -0.8660254037844388186 ) ) ;
#12385 = CARTESIAN_POINT ( 'NONE',  ( -171.4541674549778065, 121.0456171749203520, 2.431557144026069928 ) ) ;
#12386 = EDGE_LOOP ( 'NONE', ( #6874, #9981, #8390, #5058 ) ) ;
#12387 = CARTESIAN_POINT ( 'NONE',  ( -219.4906815929313950, 153.9872024941471693, 3.763993901578424062 ) ) ;
#12388 = ORIENTED_EDGE ( 'NONE', *, *, #8657, .T. ) ;
#12389 = DIRECTION ( 'NONE',  ( -0.8731965799097685110, 0.4873681696970816324, 0.000000000000000000 ) ) ;
#12390 = CARTESIAN_POINT ( 'NONE',  ( 192.9674079352396348, 50.35451258660443585, -3.442919105360563226 ) ) ;
#12391 = EDGE_LOOP ( 'NONE', ( #15231, #13248 ) ) ;
#12392 =( REPRESENTATION_RELATIONSHIP ('NONE','NONE', #3298, #11876 ) REPRESENTATION_RELATIONSHIP_WITH_TRANSFORMATION ( #13736 )SHAPE_REPRESENTATION_RELATIONSHIP( ) );
#12393 = DIRECTION ( 'NONE',  ( 0.4873681696970815769, 0.8731965799097684000, 0.000000000000000000 ) ) ;
#12394 = CARTESIAN_POINT ( 'NONE',  ( -76.50000000000004263, 19.53993994372673626, 52.49999999999997868 ) ) ;
#12395 = ADVANCED_FACE ( 'NONE', ( #7611, #8783 ), #14838, .T. ) ;
#12396 = DIRECTION ( 'NONE',  ( 0.000000000000000000, -1.000000000000000000, -6.938893903907227145E-17 ) ) ;
#12397 = ORIENTED_EDGE ( 'NONE', *, *, #5615, .F. ) ;
#12398 = EDGE_CURVE ( 'NONE', #8073, #427, #12247, .T. ) ;
#12399 = EDGE_CURVE ( 'NONE', #12092, #13079, #10739, .T. ) ;
#12400 = CIRCLE ( 'NONE', #13654, 0.5000000000000004441 ) ;
#12401 = EDGE_LOOP ( 'NONE', ( #10981, #6406, #10610, #3100 ) ) ;
#12402 = CARTESIAN_POINT ( 'NONE',  ( 14.00000000000004086, 62.13993994372673768, 15.00000000000104983 ) ) ;
#12403 = EDGE_CURVE ( 'NONE', #8789, #457, #1511, .T. ) ;
#12404 = DIRECTION ( 'NONE',  ( -0.000000000000000000, 1.000000000000000000, 1.156482317317871725E-16 ) ) ;
#12405 = VERTEX_POINT ( 'NONE', #6188 ) ;
#12406 = DIRECTION ( 'NONE',  ( 0.000000000000000000, -1.000000000000000000, -4.956352788505162775E-17 ) ) ;
#12407 = FACE_BOUND ( 'NONE', #7766, .T. ) ;
#12408 = ORIENTED_EDGE ( 'NONE', *, *, #9434, .F. ) ;
#12409 = ORIENTED_EDGE ( 'NONE', *, *, #3050, .F. ) ;
#12410 = DIRECTION ( 'NONE',  ( 0.6130913241491352528, 0.7900120431063439863, -6.390853288732736916E-17 ) ) ;
#12411 = CARTESIAN_POINT ( 'NONE',  ( 207.1131222881253393, 35.56952893079440514, -7.807171136772324438 ) ) ;
#12412 = VERTEX_POINT ( 'NONE', #14613 ) ;
#12413 = CARTESIAN_POINT ( 'NONE',  ( -70.00000000000000000, 17.53993994372673626, 47.49999999999997868 ) ) ;
#12414 = CARTESIAN_POINT ( 'NONE',  ( -155.8464059187621444, 109.5855229202700087, -4.675203989473057931 ) ) ;
#12415 = FACE_OUTER_BOUND ( 'NONE', #4902, .T. ) ;
#12416 = AXIS2_PLACEMENT_3D ( 'NONE', #9014, #15222, #12859 ) ;
#12417 = CARTESIAN_POINT ( 'NONE',  ( 165.4217645774054120, 62.57671370024034729, -0.9107274384406883749 ) ) ;
#12418 = ADVANCED_FACE ( 'NONE', ( #152 ), #6261, .T. ) ;
#12419 = ADVANCED_FACE ( 'NONE', ( #4921, #3889, #3813 ), #13430, .F. ) ;
#12420 = ORIENTED_EDGE ( 'NONE', *, *, #2507, .F. ) ;
#12421 = CARTESIAN_POINT ( 'NONE',  ( -216.9004380970166039, 154.5406409916104735, -0.03430832140138441455 ) ) ;
#12422 = CARTESIAN_POINT ( 'NONE',  ( -209.9898587843626956, 141.8296236499265035, -5.230826428279598872 ) ) ;
#12423 = CARTESIAN_POINT ( 'NONE',  ( -157.6477983077465694, 110.1970436846185066, 0.000000000000000000 ) ) ;
#12424 = EDGE_LOOP ( 'NONE', ( #9390, #1826 ) ) ;
#12425 = CARTESIAN_POINT ( 'NONE',  ( -205.9652191273047777, 131.2378527988410326, 3.478895870929496148 ) ) ;
#12426 = CARTESIAN_POINT ( 'NONE',  ( 193.1436046380909772, 46.22450523326372007, -4.738359826975481859 ) ) ;
#12427 = CIRCLE ( 'NONE', #2611, 1.699999999999998401 ) ;
#12428 = ORIENTED_EDGE ( 'NONE', *, *, #7640, .T. ) ;
#12429 = EDGE_CURVE ( 'NONE', #9960, #627, #4422, .T. ) ;
#12430 = CIRCLE ( 'NONE', #9935, 2.749999999999999112 ) ;
#12431 = CARTESIAN_POINT ( 'NONE',  ( -85.27455057502459113, 65.19100426474074084, 9.975000000000001421 ) ) ;
#12432 = FACE_BOUND ( 'NONE', #3043, .T. ) ;
#12433 = DIRECTION ( 'NONE',  ( 0.000000000000000000, 0.000000000000000000, 1.000000000000000000 ) ) ;
#12434 = CIRCLE ( 'NONE', #10695, 1.499999999999994449 ) ;
#12435 = PLANE ( 'NONE',  #14449 ) ;
#12436 = ORIENTED_EDGE ( 'NONE', *, *, #2176, .F. ) ;
#12437 = CARTESIAN_POINT ( 'NONE',  ( 172.5293059057019889, 61.25683321636181233, 0.000000000000000000 ) ) ;
#12438 = CONICAL_SURFACE ( 'NONE', #2113, 3.525000000000000355, 0.7853981633974482790 ) ;
#12439 = CARTESIAN_POINT ( 'NONE',  ( -177.5673841713239085, 132.5493133318365437, 5.434754235172600367 ) ) ;
#12440 = DIRECTION ( 'NONE',  ( -0.000000000000000000, 1.000000000000000000, -0.000000000000000000 ) ) ;
#12441 = CARTESIAN_POINT ( 'NONE',  ( -157.2827495303359626, 110.9803135124890616, -4.829560219627786921 ) ) ;
#12442 = ORIENTED_EDGE ( 'NONE', *, *, #12204, .T. ) ;
#12444 = AXIS2_PLACEMENT_3D ( 'NONE', #4466, #3067, #668 ) ;
#12443 = CARTESIAN_POINT ( 'NONE',  ( 190.5000000000000853, 17.53993994372673271, 52.49999999999997868 ) ) ;
#12445 = ORIENTED_EDGE ( 'NONE', *, *, #2573, .T. ) ;
#12446 = EDGE_CURVE ( 'NONE', #2049, #9261, #4160, .T. ) ;
#12447 = ORIENTED_EDGE ( 'NONE', *, *, #12648, .T. ) ;
#12448 = LINE ( 'NONE', #1637, #3007 ) ;
#12449 = CARTESIAN_POINT ( 'NONE',  ( 51.39999999999999858, 0.000000000000000000, 0.000000000000000000 ) ) ;
#12450 = CONICAL_SURFACE ( 'NONE', #10947, 3.525000000000002132, 0.7853981633974482790 ) ;
#12451 = PRESENTATION_STYLE_ASSIGNMENT (( #9870 ) ) ;
#12452 =( LENGTH_UNIT ( ) NAMED_UNIT ( * ) SI_UNIT ( .MILLI., .METRE. ) );
#12453 = DIRECTION ( 'NONE',  ( 0.000000000000000000, -0.1391731009600641333, -0.9902680687415704730 ) ) ;
#12454 = CARTESIAN_POINT ( 'NONE',  ( -221.0392844523455267, 151.2126373818634306, -2.672071523003486160 ) ) ;
#12455 = CARTESIAN_POINT ( 'NONE',  ( -192.3703904092303105, 140.8200239622036918, 5.434754235172604808 ) ) ;
#12456 = AXIS2_PLACEMENT_3D ( 'NONE', #8068, #8231, #2043 ) ;
#12457 = ORIENTED_EDGE ( 'NONE', *, *, #11934, .F. ) ;
#12458 = FACE_OUTER_BOUND ( 'NONE', #1763, .T. ) ;
#12459 = CARTESIAN_POINT ( 'NONE',  ( 205.5168546899054434, 47.82311440310952833, -1.064259200291542529 ) ) ;
#12460 = DIRECTION ( 'NONE',  ( -1.000000000000000000, 0.000000000000000000, 0.000000000000000000 ) ) ;
#12461 = VERTEX_POINT ( 'NONE', #2706 ) ;
#12462 = CARTESIAN_POINT ( 'NONE',  ( -221.6258104990438937, 150.1617839001448260, 7.894136746929314441 ) ) ;
#12463 = ORIENTED_EDGE ( 'NONE', *, *, #3894, .F. ) ;
#12464 = CARTESIAN_POINT ( 'NONE',  ( -168.0753201600388422, 127.0993524933591630, -0.6766640714057908790 ) ) ;
#12465 = PLANE ( 'NONE',  #11144 ) ;
#12466 = VERTEX_POINT ( 'NONE', #2867 ) ;
#12467 = DIRECTION ( 'NONE',  ( -0.000000000000000000, -1.000000000000000000, -6.938893903907227145E-17 ) ) ;
#12468 = FACE_OUTER_BOUND ( 'NONE', #352, .T. ) ;
#12469 = EDGE_CURVE ( 'NONE', #10853, #8326, #5936, .T. ) ;
#12470 = CARTESIAN_POINT ( 'NONE',  ( -76.50000000000001421, 19.53993994372674692, -17.50000000000002487 ) ) ;
#12471 = VERTEX_POINT ( 'NONE', #386 ) ;
#12472 = CARTESIAN_POINT ( 'NONE',  ( 200.1062858801502671, 40.86394065090232175, -26.99999999999999645 ) ) ;
#12473 = ORIENTED_EDGE ( 'NONE', *, *, #5362, .F. ) ;
#12474 = DIRECTION ( 'NONE',  ( 0.000000000000000000, 0.000000000000000000, 1.000000000000000000 ) ) ;
#12475 = CARTESIAN_POINT ( 'NONE',  ( 14.00000000000004086, 59.53993994372674337, 16.70000000000104734 ) ) ;
#12476 = EDGE_LOOP ( 'NONE', ( #7632, #11209, #14343, #2138, #8532, #12342 ) ) ;
#12477 = CARTESIAN_POINT ( 'NONE',  ( -85.27455057502459113, 65.19100426474074084, 9.975000000000001421 ) ) ;
#12478 = VECTOR ( 'NONE', #10611, 1000.000000000000000 ) ;
#12479 = CARTESIAN_POINT ( 'NONE',  ( 14.00000000000004086, 62.13993994372673768, 18.50000000000105160 ) ) ;
#12480 = ORIENTED_EDGE ( 'NONE', *, *, #4482, .T. ) ;
#12481 = ORIENTED_EDGE ( 'NONE', *, *, #5985, .T. ) ;
#12482 = DIRECTION ( 'NONE',  ( 0.000000000000000000, 0.000000000000000000, -1.000000000000000000 ) ) ;
#12483 = CARTESIAN_POINT ( 'NONE',  ( 202.3883256910358739, 32.65987148549056229, -8.116337980372584582 ) ) ;
#12484 = EDGE_CURVE ( 'NONE', #7800, #12769, #11158, .T. ) ;
#12485 = ORIENTED_EDGE ( 'NONE', *, *, #14295, .T. ) ;
#12486 = DIRECTION ( 'NONE',  ( 1.000000000000000000, -2.751328491981765035E-32, 3.965082230804130220E-16 ) ) ;
#12487 = CYLINDRICAL_SURFACE ( 'NONE', #2273, 3.499999999999999556 ) ;
#12488 = CARTESIAN_POINT ( 'NONE',  ( -76.00000000000004263, 15.53993994372673626, 52.49999999999997868 ) ) ;
#12489 = DIRECTION ( 'NONE',  ( -0.000000000000000000, -0.000000000000000000, 1.000000000000000000 ) ) ;
#12490 = DIRECTION ( 'NONE',  ( 1.000000000000000000, 0.000000000000000000, 0.000000000000000000 ) ) ;
#12491 = AXIS2_PLACEMENT_3D ( 'NONE', #1668, #8000, #12709 ) ;
#12492 = AXIS2_PLACEMENT_3D ( 'NONE', #7878, #10310, #1774 ) ;
#12493 = CARTESIAN_POINT ( 'NONE',  ( -110.0000000000000426, 56.53993994372675047, 25.00000000000000000 ) ) ;
#12494 = ORIENTED_EDGE ( 'NONE', *, *, #8380, .T. ) ;
#12495 = DIRECTION ( 'NONE',  ( 0.000000000000000000, 0.000000000000000000, -1.000000000000000000 ) ) ;
#12496 = DIRECTION ( 'NONE',  ( 1.000000000000000000, 2.775557561562892929E-15, 0.000000000000000000 ) ) ;
#12497 = CARTESIAN_POINT ( 'NONE',  ( -223.5232045190763301, 146.7623046726374980, -4.689260562946596878 ) ) ;
#12498 = DIRECTION ( 'NONE',  ( -0.000000000000000000, 0.9902680687415713612, -0.1391731009600582492 ) ) ;
#12499 = ORIENTED_EDGE ( 'NONE', *, *, #9312, .T. ) ;
#12500 = CARTESIAN_POINT ( 'NONE',  ( -213.7863261933728154, 135.0464837791089963, 5.434137442415932995 ) ) ;
#12501 = CARTESIAN_POINT ( 'NONE',  ( 207.1194509196011495, 46.14302886020001182, -1.185720282267065828 ) ) ;
#12502 = ADVANCED_FACE ( 'NONE', ( #5226 ), #8977, .F. ) ;
#12503 = EDGE_LOOP ( 'NONE', ( #4829, #11683, #7610, #3885, #1348, #4519, #2318, #12481, #615 ) ) ;
#12504 = EDGE_CURVE ( 'NONE', #14396, #13094, #14506, .T. ) ;
#12505 = EDGE_CURVE ( 'NONE', #935, #158, #14751, .T. ) ;
#12506 = CIRCLE ( 'NONE', #3181, 3.500000000000003109 ) ;
#12507 = DIRECTION ( 'NONE',  ( -0.000000000000000000, -0.000000000000000000, -1.000000000000000000 ) ) ;
#12508 = FACE_OUTER_BOUND ( 'NONE', #5695, .T. ) ;
#12509 = CARTESIAN_POINT ( 'NONE',  ( 172.5293059057019889, 61.25683321636181233, 10.00000000000000178 ) ) ;
#12510 = CARTESIAN_POINT ( 'NONE',  ( -76.50000000000001421, -181.3058001507315566, 84.88378295107885663 ) ) ;
#12511 = VECTOR ( 'NONE', #9475, 1000.000000000000000 ) ;
#12512 = ORIENTED_EDGE ( 'NONE', *, *, #11962, .T. ) ;
#12513 = CARTESIAN_POINT ( 'NONE',  ( -152.4086188282879277, 107.2728346664360259, 5.000000000000004441 ) ) ;
#12514 = CARTESIAN_POINT ( 'NONE',  ( -172.5511497006709192, 129.7930440361603246, 5.430596897033706405 ) ) ;
#12515 = DIRECTION ( 'NONE',  ( 1.000000000000000000, 0.000000000000000000, 0.000000000000000000 ) ) ;
#12516 = DIRECTION ( 'NONE',  ( -0.000000000000000000, 0.000000000000000000, 1.000000000000000000 ) ) ;
#12517 = EDGE_LOOP ( 'NONE', ( #4144, #5345 ) ) ;
#12518 = DIRECTION ( 'NONE',  ( 0.000000000000000000, 0.000000000000000000, -1.000000000000000000 ) ) ;
#12519 = ORIENTED_EDGE ( 'NONE', *, *, #5368, .F. ) ;
#12520 = EDGE_LOOP ( 'NONE', ( #5202, #4245, #8662, #7614 ) ) ;
#12521 = LINE ( 'NONE', #7574, #14583 ) ;
#12522 = DIRECTION ( 'NONE',  ( -0.000000000000000000, 0.000000000000000000, 1.000000000000000000 ) ) ;
#12523 = PLANE ( 'NONE',  #1847 ) ;
#12524 = CARTESIAN_POINT ( 'NONE',  ( -157.6477983077465694, 110.1970436846185066, 5.000000000000000000 ) ) ;
#12525 = CARTESIAN_POINT ( 'NONE',  ( -218.4739499160498042, 155.8088368932420167, 1.364465161875672239 ) ) ;
#12526 = ORIENTED_EDGE ( 'NONE', *, *, #13028, .F. ) ;
#12527 = ADVANCED_FACE ( 'NONE', ( #7689 ), #5469, .F. ) ;
#12528 = CARTESIAN_POINT ( 'NONE',  ( 172.5293059057019889, 61.25683321636181233, 5.000000000000000000 ) ) ;
#12529 = ADVANCED_FACE ( 'NONE', ( #1895 ), #11385, .F. ) ;
#12530 = DIRECTION ( 'NONE',  ( -3.965082230804130220E-16, -0.000000000000000000, -1.000000000000000000 ) ) ;
#12531 = CARTESIAN_POINT ( 'NONE',  ( 215.1062858801516882, 25.86394065090268057, 13.00000000000000178 ) ) ;
#12532 = ORIENTED_EDGE ( 'NONE', *, *, #8157, .F. ) ;
#12533 = CIRCLE ( 'NONE', #7521, 0.5000000000000004441 ) ;
#12534 = CARTESIAN_POINT ( 'NONE',  ( -219.9184004181287264, 153.2208770782757767, 5.686502709355995222 ) ) ;
#12535 = EDGE_LOOP ( 'NONE', ( #12526, #13252, #7208, #3252, #8468 ) ) ;
#12536 = PLANE ( 'NONE',  #8812 ) ;
#12537 = CARTESIAN_POINT ( 'NONE',  ( 5.196152422706632024, 9.000000000000003553, 5.000000000000000000 ) ) ;
#12538 = VERTEX_POINT ( 'NONE', #5386 ) ;
#12539 = CARTESIAN_POINT ( 'NONE',  ( -108.0000000000000568, 59.53993994372674337, 10.00000000000000178 ) ) ;
#12540 = CARTESIAN_POINT ( 'NONE',  ( 2.000000000000000000, -3.175426480542940411, 0.000000000000000000 ) ) ;
#12541 = PRODUCT_DEFINITION_SHAPE ( 'NONE', 'NONE',  #6143 ) ;
#12542 = AXIS2_PLACEMENT_3D ( 'NONE', #2200, #7032, #1558 ) ;
#12543 = CARTESIAN_POINT ( 'NONE',  ( 2.000000000000000000, 1.587713240271468207, -2.750000000000000000 ) ) ;
#12544 = ORIENTED_EDGE ( 'NONE', *, *, #6535, .F. ) ;
#12545 = VECTOR ( 'NONE', #7087, 999.9999999999998863 ) ;
#12546 = SHAPE_REPRESENTATION ( 'nut M10', ( #12337 ), #9054 ) ;
#12547 = EDGE_CURVE ( 'NONE', #8130, #319, #9230, .T. ) ;
#12548 = PRODUCT_CONTEXT ( 'NONE', #5649, 'mechanical' ) ;
#12549 = ORIENTED_EDGE ( 'NONE', *, *, #1025, .T. ) ;
#12550 = DIRECTION ( 'NONE',  ( -0.000000000000000000, -0.000000000000000000, 1.000000000000000000 ) ) ;
#12551 = ORIENTED_EDGE ( 'NONE', *, *, #9134, .F. ) ;
#12552 = CARTESIAN_POINT ( 'NONE',  ( -64.00000000000002842, -179.3058001507315566, 65.31842631998698323 ) ) ;
#12553 = CARTESIAN_POINT ( 'NONE',  ( -35.99999999999995026, 64.53993994372673626, 15.00000000000139977 ) ) ;
#12554 = ORIENTED_EDGE ( 'NONE', *, *, #5274, .F. ) ;
#12555 = ORIENTED_EDGE ( 'NONE', *, *, #855, .F. ) ;
#12556 = DIRECTION ( 'NONE',  ( 0.000000000000000000, 0.000000000000000000, -1.000000000000000000 ) ) ;
#12557 = EDGE_CURVE ( 'NONE', #6601, #10382, #6664, .T. ) ;
#12558 = AXIS2_PLACEMENT_3D ( 'NONE', #3752, #5095, #1446 ) ;
#12559 = ORIENTED_EDGE ( 'NONE', *, *, #948, .T. ) ;
#12560 = CARTESIAN_POINT ( 'NONE',  ( 177.5000000000000853, 17.53993994372674692, -17.50000000000002487 ) ) ;
#12561 = LINE ( 'NONE', #8879, #7078 ) ;
#12562 = DIRECTION ( 'NONE',  ( -1.000000000000000000, -0.000000000000000000, -0.000000000000000000 ) ) ;
#12563 = DIRECTION ( 'NONE',  ( 0.000000000000000000, 0.000000000000000000, 1.000000000000000000 ) ) ;
#12564 = CARTESIAN_POINT ( 'NONE',  ( 64.00000000000005684, 59.53993994372674337, 16.70000000000069207 ) ) ;
#12565 = AXIS2_PLACEMENT_3D ( 'NONE', #6155, #8377, #3464 ) ;
#12566 = ADVANCED_FACE ( 'NONE', ( #10207, #699, #3018 ), #4347, .T. ) ;
#12567 = DIRECTION ( 'NONE',  ( 0.000000000000000000, 0.000000000000000000, -1.000000000000000000 ) ) ;
#12568 = ORIENTED_EDGE ( 'NONE', *, *, #2084, .T. ) ;
#12569 = CARTESIAN_POINT ( 'NONE',  ( -76.50000000000001421, -178.7362136002515172, -17.68580191161595394 ) ) ;
#12570 = CARTESIAN_POINT ( 'NONE',  ( -192.1661132380199604, 141.2048990416207630, 1.515441477536284332 ) ) ;
#12571 = CARTESIAN_POINT ( 'NONE',  ( -64.00000000000002842, -179.8058001507315566, 52.19066787724494816 ) ) ;
#12572 = ORIENTED_EDGE ( 'NONE', *, *, #537, .F. ) ;
#12573 = CARTESIAN_POINT ( 'NONE',  ( -173.9416064256852508, 115.8726071073731987, 3.216677072105399660 ) ) ;
#12574 = CARTESIAN_POINT ( 'NONE',  ( 188.3636875860777593, 42.62859381388609137, -4.500015676459212521 ) ) ;
#12575 = ORIENTED_EDGE ( 'NONE', *, *, #9098, .T. ) ;
#12576 = CIRCLE ( 'NONE', #12078, 0.5000000000000001110 ) ;
#12577 = AXIS2_PLACEMENT_3D ( 'NONE', #8951, #3099, #5153 ) ;
#12578 = DIRECTION ( 'NONE',  ( -0.000000000000000000, -0.000000000000000000, 1.000000000000000000 ) ) ;
#12579 = LINE ( 'NONE', #10385, #2936 ) ;
#12580 = EDGE_CURVE ( 'NONE', #10761, #4605, #3415, .T. ) ;
#12581 = CARTESIAN_POINT ( 'NONE',  ( -127.3091761562077409, 106.2673160437096413, 5.000000000000000000 ) ) ;
#12582 = AXIS2_PLACEMENT_3D ( 'NONE', #12670, #6701, #13943 ) ;
#12583 = CIRCLE ( 'NONE', #15353, 0.5000000000000004441 ) ;
#12584 = CIRCLE ( 'NONE', #5796, 1.499999999999997780 ) ;
#12585 = CARTESIAN_POINT ( 'NONE',  ( 170.9049199631132581, 71.79964605558720336, -0.9107274384406883749 ) ) ;
#12587 = EDGE_CURVE ( 'NONE', #7467, #12158, #12001, .T. ) ;
#12586 = PRODUCT_DEFINITION ( 'UNKNOWN', '', #2745, #15279 ) ;
#12588 = ADVANCED_FACE ( 'NONE', ( #6737 ), #890, .T. ) ;
#12589 = VERTEX_POINT ( 'NONE', #1973 ) ;
#12590 = AXIS2_PLACEMENT_3D ( 'NONE', #10219, #7704, #8797 ) ;
#12591 = CARTESIAN_POINT ( 'NONE',  ( 224.0000000000000853, 19.53993994372674337, 9.999999999999998224 ) ) ;
#12592 = CARTESIAN_POINT ( 'NONE',  ( -212.8994228580217509, 136.6308034654096559, 7.918248976830621011 ) ) ;
#12593 = FACE_OUTER_BOUND ( 'NONE', #4353, .T. ) ;
#12594 = EDGE_CURVE ( 'NONE', #12968, #1955, #7849, .T. ) ;
#12595 = CARTESIAN_POINT ( 'NONE',  ( -157.6477983077465694, 110.1970436846185208, -4.548387523817069678 ) ) ;
#12596 = ORIENTED_EDGE ( 'NONE', *, *, #14574, .F. ) ;
#12597 = LINE ( 'NONE', #5346, #3553 ) ;
#12598 = ORIENTED_EDGE ( 'NONE', *, *, #11478, .T. ) ;
#12599 = VERTEX_POINT ( 'NONE', #783 ) ;
#12600 = AXIS2_PLACEMENT_3D ( 'NONE', #9345, #10602, #9416 ) ;
#12601 = LINE ( 'NONE', #429, #13571 ) ;
#12602 = CARTESIAN_POINT ( 'NONE',  ( 175.9483885134608272, -179.3058001507315566, 84.88378295107887084 ) ) ;
#12603 = AXIS2_PLACEMENT_3D ( 'NONE', #608, #15281, #2117 ) ;
#12604 = B_SPLINE_CURVE_WITH_KNOTS ( 'NONE', 3,
 ( #10851, #550, #630, #11233, #1824, #10208 ),
 .UNSPECIFIED., .F., .F.,
 ( 4, 2, 4 ),
 ( 0.001606744326298690335, 0.002406996759593249199, 0.003207249192887807847 ),
 .UNSPECIFIED. ) ;
#12605 = AXIS2_PLACEMENT_3D ( 'NONE', #10157, #3984, #1851 ) ;
#12606 = DIRECTION ( 'NONE',  ( -0.4873681696970814659, -0.8731965799097686221, 0.000000000000000000 ) ) ;
#12607 = DIRECTION ( 'NONE',  ( 1.000000000000000000, -2.751328491981765035E-32, 3.965082230804130220E-16 ) ) ;
#12608 = CARTESIAN_POINT ( 'NONE',  ( -220.0724991394466485, 152.9447850296163836, -1.223998976583901444 ) ) ;
#12609 = LINE ( 'NONE', #15045, #4684 ) ;
#12610 = EDGE_CURVE ( 'NONE', #12371, #12789, #9476, .T. ) ;
#12611 = DIRECTION ( 'NONE',  ( -0.000000000000000000, -0.000000000000000000, 1.000000000000000000 ) ) ;
#12612 = PRODUCT_DEFINITION_CONTEXT ( 'detailed design', #8885, 'design' ) ;
#12613 = AXIS2_PLACEMENT_3D ( 'NONE', #10195, #9013, #3879 ) ;
#12614 = CARTESIAN_POINT ( 'NONE',  ( 164.0000000000000568, 64.53993994372673626, 15.00000000000000355 ) ) ;
#12615 = VECTOR ( 'NONE', #14884, 1000.000000000000000 ) ;
#12616 = CARTESIAN_POINT ( 'NONE',  ( 194.8381067511959372, 47.88228248201940573, -3.436395123936771601 ) ) ;
#12617 = DIRECTION ( 'NONE',  ( -0.000000000000000000, -0.000000000000000000, -1.000000000000000000 ) ) ;
#12618 = VERTEX_POINT ( 'NONE', #5301 ) ;
#12619 = EDGE_CURVE ( 'NONE', #11858, #15074, #15229, .T. ) ;
#12620 = CARTESIAN_POINT ( 'NONE',  ( -219.8231187948979652, 153.3915890629854744, 5.390158053389423110 ) ) ;
#12621 = ORIENTED_EDGE ( 'NONE', *, *, #1267, .T. ) ;
#12622 = DIRECTION ( 'NONE',  ( -0.000000000000000000, 1.000000000000000000, 0.000000000000000000 ) ) ;
#12623 = CARTESIAN_POINT ( 'NONE',  ( -63.50000000000002842, 19.53993994372674337, 24.99999999999999645 ) ) ;
#12624 = ORIENTED_EDGE ( 'NONE', *, *, #12225, .F. ) ;
#12625 = CARTESIAN_POINT ( 'NONE',  ( -5.196152422706630247, -9.000000000000005329, 5.000000000000000000 ) ) ;
#12626 = CARTESIAN_POINT ( 'NONE',  ( -70.00000000000000000, 19.53993994372673626, 45.99999999999998579 ) ) ;
#12627 = AXIS2_PLACEMENT_3D ( 'NONE', #5812, #9686, #14320 ) ;
#12628 = EDGE_CURVE ( 'NONE', #14434, #7029, #11466, .T. ) ;
#12629 = CIRCLE ( 'NONE', #800, 0.9999999999999991118 ) ;
#12630 = DIRECTION ( 'NONE',  ( -0.000000000000000000, -0.000000000000000000, 1.000000000000000000 ) ) ;
#12631 = VERTEX_POINT ( 'NONE', #4114 ) ;
#12632 = ORIENTED_EDGE ( 'NONE', *, *, #11584, .F. ) ;
#12633 = CARTESIAN_POINT ( 'NONE',  ( 208.8313558426846157, 41.97310978343666932, 0.1351797820921298021 ) ) ;
#12634 = LINE ( 'NONE', #308, #936 ) ;
#12635 = ORIENTED_EDGE ( 'NONE', *, *, #2924, .T. ) ;
#12636 = CARTESIAN_POINT ( 'NONE',  ( 190.0000000000000568, 15.53993994372674159, 9.617930870223352358 ) ) ;
#12637 = AXIS2_PLACEMENT_3D ( 'NONE', #1322, #6231, #8524 ) ;
#12638 = CARTESIAN_POINT ( 'NONE',  ( 64.00000000000005684, 59.53993994372674337, 13.30000000000070948 ) ) ;
#12639 = VERTEX_POINT ( 'NONE', #8950 ) ;
#12640 = ORIENTED_EDGE ( 'NONE', *, *, #3183, .F. ) ;
#12641 = VECTOR ( 'NONE', #6808, 1000.000000000000000 ) ;
#12642 = FACE_OUTER_BOUND ( 'NONE', #1743, .T. ) ;
#12643 = ORIENTED_EDGE ( 'NONE', *, *, #11651, .T. ) ;
#12644 = CARTESIAN_POINT ( 'NONE',  ( 193.0950460371283839, 35.57958264137020876, -2.685405722344195389 ) ) ;
#12645 = PLANE ( 'NONE',  #10079 ) ;
#12646 = CYLINDRICAL_SURFACE ( 'NONE', #11851, 17.06579782980005433 ) ;
#12647 = FACE_OUTER_BOUND ( 'NONE', #5845, .T. ) ;
#12648 = EDGE_CURVE ( 'NONE', #12769, #10711, #9990, .T. ) ;
#12649 = FACE_OUTER_BOUND ( 'NONE', #13271, .T. ) ;
#12650 = DIRECTION ( 'NONE',  ( 0.000000000000000000, 0.000000000000000000, 1.000000000000000000 ) ) ;
#12651 = EDGE_LOOP ( 'NONE', ( #12353, #9107, #10442, #940 ) ) ;
#12652 = LINE ( 'NONE', #4130, #10220 ) ;
#12653 = CARTESIAN_POINT ( 'NONE',  ( -180.1141531658810777, 134.0357633396332915, -0.4547266291960706530 ) ) ;
#12654 = CARTESIAN_POINT ( 'NONE',  ( 190.0000000000000568, 15.03993994372673981, -3.075184203610571654 ) ) ;
#12655 = ORIENTED_EDGE ( 'NONE', *, *, #8743, .T. ) ;
#12656 = CARTESIAN_POINT ( 'NONE',  ( -176.6594047394515314, 116.7136007993067324, 3.281269053145625225 ) ) ;
#12657 = CARTESIAN_POINT ( 'NONE',  ( 190.7182813446581235, 33.54593944905032998, -7.256469109801526152 ) ) ;
#12658 = VERTEX_POINT ( 'NONE', #12552 ) ;
#12660 =( GEOMETRIC_REPRESENTATION_CONTEXT ( 3 ) GLOBAL_UNCERTAINTY_ASSIGNED_CONTEXT ( ( #9128 ) ) GLOBAL_UNIT_ASSIGNED_CONTEXT ( ( #13081, #7113, #13712 ) ) REPRESENTATION_CONTEXT ( 'NONE', 'WORKASPACE' ) );
#12659 = VECTOR ( 'NONE', #5864, 999.9999999999997726 ) ;
#12661 = EDGE_CURVE ( 'NONE', #4947, #3997, #4261, .T. ) ;
#12662 = LINE ( 'NONE', #2004, #14592 ) ;
#12663 = CARTESIAN_POINT ( 'NONE',  ( -220.3531759299249302, 148.3382346779569616, 2.431557144026069928 ) ) ;
#12664 = DIRECTION ( 'NONE',  ( 1.000000000000000000, 0.000000000000000000, 0.000000000000000000 ) ) ;
#12665 = CARTESIAN_POINT ( 'NONE',  ( -156.6477983077465410, 110.1970436846185066, 0.000000000000000000 ) ) ;
#12666 = VERTEX_POINT ( 'NONE', #628 ) ;
#12667 = CARTESIAN_POINT ( 'NONE',  ( -5.196152422706630247, -9.000000000000005329, 5.000000000000000000 ) ) ;
#12668 = CARTESIAN_POINT ( 'NONE',  ( -203.7296541848517109, 135.3294987143146955, 9.577123744044227394 ) ) ;
#12669 = CYLINDRICAL_SURFACE ( 'NONE', #13044, 1.700000000000007061 ) ;
#12670 = CARTESIAN_POINT ( 'NONE',  ( 2.000000000000000000, 1.587713240271468207, -2.750000000000000000 ) ) ;
#12671 = VERTEX_POINT ( 'NONE', #5768 ) ;
#12672 = ADVANCED_FACE ( 'NONE', ( #4499 ), #10748, .F. ) ;
#12673 = AXIS2_PLACEMENT_3D ( 'NONE', #4811, #9631, #8527 ) ;
#12674 = DIRECTION ( 'NONE',  ( -0.000000000000000000, 1.000000000000000000, -0.000000000000000000 ) ) ;
#12675 = EDGE_LOOP ( 'NONE', ( #1209, #12023 ) ) ;
#12676 = ORIENTED_EDGE ( 'NONE', *, *, #6897, .T. ) ;
#12677 = CARTESIAN_POINT ( 'NONE',  ( 122.5806775638430253, 45.00321902537314145, 7.600000000000002309 ) ) ;
#12678 = LINE ( 'NONE', #5351, #2733 ) ;
#12679 = EDGE_CURVE ( 'NONE', #1214, #14616, #9335, .T. ) ;
#12680 =( NAMED_UNIT ( * ) SI_UNIT ( $, .STERADIAN. ) SOLID_ANGLE_UNIT ( ) );
#12681 = CARTESIAN_POINT ( 'NONE',  ( -169.2966169123036480, 124.9112076504258368, 8.722866747349085514 ) ) ;
#12682 = CARTESIAN_POINT ( 'NONE',  ( -219.8602732318529434, 153.3250210569181320, -0.6604898282866703552 ) ) ;
#12683 = CONICAL_SURFACE ( 'NONE', #12180, 1.219500000000000028, 0.7853981633974552734 ) ;
#12684 = ADVANCED_FACE ( 'NONE', ( #10511 ), #15385, .F. ) ;
#12685 = LINE ( 'NONE', #4317, #5452 ) ;
#12686 = APPLICATION_CONTEXT ( 'automotive_design' ) ;
#12687 = DIRECTION ( 'NONE',  ( -1.000000000000000000, 0.000000000000000000, 0.000000000000000000 ) ) ;
#12688 = DIRECTION ( 'NONE',  ( -0.000000000000000000, 0.9902680687415712502, 0.1391731009600586100 ) ) ;
#12689 = CARTESIAN_POINT ( 'NONE',  ( -63.50000000000002842, 16.03993994372673981, 24.94742576086838781 ) ) ;
#12690 = DIRECTION ( 'NONE',  ( 0.000000000000000000, 0.000000000000000000, 1.000000000000000000 ) ) ;
#12691 = EDGE_LOOP ( 'NONE', ( #1023, #14044, #10913, #2750, #2382, #8829 ) ) ;
#12692 = AXIS2_PLACEMENT_3D ( 'NONE', #1156, #6145, #3380 ) ;
#12693 = VERTEX_POINT ( 'NONE', #941 ) ;
#12694 = DIRECTION ( 'NONE',  ( 0.000000000000000000, 0.000000000000000000, -1.000000000000000000 ) ) ;
#12695 = FACE_BOUND ( 'NONE', #2158, .T. ) ;
#12696 = EDGE_CURVE ( 'NONE', #14095, #2217, #10990, .T. ) ;
#12698 = DIRECTION ( 'NONE',  ( 1.000000000000000000, 0.000000000000000000, 0.000000000000000000 ) ) ;
#12697 = VECTOR ( 'NONE', #3982, 1000.000000000000000 ) ;
#12699 = ADVANCED_FACE ( 'NONE', ( #2134 ), #865, .F. ) ;
#12700 = CARTESIAN_POINT ( 'NONE',  ( -63.50000000000002842, -179.8058001507315566, -30.31842631998718574 ) ) ;
#12701 = DIRECTION ( 'NONE',  ( 3.965082230804130220E-16, 4.956352788505162775E-17, -1.000000000000000000 ) ) ;
#12702 = FACE_BOUND ( 'NONE', #7039, .T. ) ;
#12703 = EDGE_LOOP ( 'NONE', ( #2127, #12632, #2133, #8128 ) ) ;
#12704 = ITEM_DEFINED_TRANSFORMATION ( 'NONE', 'NONE', #9804,  #12337 ) ;
#12705 = ORIENTED_EDGE ( 'NONE', *, *, #13495, .F. ) ;
#12706 = CARTESIAN_POINT ( 'NONE',  ( 209.6240687314160880, 33.75364762868482416, -9.385773361654676350 ) ) ;
#12707 = PLANE ( 'NONE',  #10812 ) ;
#12708 = ORIENTED_EDGE ( 'NONE', *, *, #15572, .T. ) ;
#12709 = DIRECTION ( 'NONE',  ( 0.000000000000000000, 0.000000000000000000, -1.000000000000000000 ) ) ;
#12710 = ADVANCED_FACE ( 'NONE', ( #15533, #8396, #13095 ), #11775, .T. ) ;
#12711 = DIRECTION ( 'NONE',  ( 1.000000000000000000, 0.000000000000000000, 0.000000000000000000 ) ) ;
#12712 = ORIENTED_EDGE ( 'NONE', *, *, #15474, .T. ) ;
#12713 = ORIENTED_EDGE ( 'NONE', *, *, #2003, .F. ) ;
#12714 = CARTESIAN_POINT ( 'NONE',  ( 0.000000000000000000, 0.000000000000000000, 0.000000000000000000 ) ) ;
#12715 = AXIS2_PLACEMENT_3D ( 'NONE', #10014, #8744, #7725 ) ;
#12716 = ORIENTED_EDGE ( 'NONE', *, *, #11565, .T. ) ;
#12717 = CARTESIAN_POINT ( 'NONE',  ( 201.3139613293953971, 49.56665511821758230, -6.809528532989353344 ) ) ;
#12718 = CARTESIAN_POINT ( 'NONE',  ( 164.0000000000000568, 64.53993994372673626, 16.70000000000000995 ) ) ;
#12719 = CARTESIAN_POINT ( 'NONE',  ( -70.00000000000000000, 19.53993994372673626, 47.49999999999997868 ) ) ;
#12720 = CARTESIAN_POINT ( 'NONE',  ( -110.0000000000000426, 19.53993994372674337, 24.99999999999999645 ) ) ;
#12721 = CARTESIAN_POINT ( 'NONE',  ( 70.26535645333922275, 38.79159067395544014, 10.00000000000000178 ) ) ;
#12722 = AXIS2_PLACEMENT_3D ( 'NONE', #7144, #15321, #4675 ) ;
#12723 = DIRECTION ( 'NONE',  ( 0.9296197478520975555, 0.3660421972118350631, -0.04266420354037653295 ) ) ;
#12724 = ADVANCED_FACE ( 'NONE', ( #11701 ), #9733, .T. ) ;
#12725 = EDGE_CURVE ( 'NONE', #2355, #13002, #6959, .T. ) ;
#12726 = ORIENTED_EDGE ( 'NONE', *, *, #5142, .F. ) ;
#12727 = CARTESIAN_POINT ( 'NONE',  ( -34.79899788034579444, 48.72489408690345414, 7.600000000000002309 ) ) ;
#12728 = CARTESIAN_POINT ( 'NONE',  ( -168.3602667112202766, 125.8948777600411830, -3.002243219525047024 ) ) ;
#12729 = LINE ( 'NONE', #4286, #9311 ) ;
#12730 = ORIENTED_EDGE ( 'NONE', *, *, #14936, .T. ) ;
#12731 = CARTESIAN_POINT ( 'NONE',  ( -200.9686762702122849, 128.5620043109015853, -0.4555467707853345649 ) ) ;
#12732 = UNCERTAINTY_MEASURE_WITH_UNIT (LENGTH_MEASURE( 1.000000000000000082E-05 ), #13281, 'distance_accuracy_value', 'NONE');
#12733 = CARTESIAN_POINT ( 'NONE',  ( 209.5435894037482285, 33.63601521402413397, -0.2471466635189603911 ) ) ;
#12734 = VERTEX_POINT ( 'NONE', #7045 ) ;
#12735 = B_SPLINE_CURVE_WITH_KNOTS ( 'NONE', 3,
 ( #15507, #6136, #1073, #6062, #4706, #9527, #5233, #13382, #8587, #10879, #4872, #395, #13057, #11978, #8511, #8440, #12127 ),
 .UNSPECIFIED., .F., .F.,
 ( 4, 2, 2, 2, 2, 2, 3, 4 ),
 ( 0.04448509752560573377, 0.2455027589669699362, 0.3041813370740077405, 0.5308033955276699745, 0.6372805264318514018, 0.8233339832829627003, 0.9999999999999998890, 1.159754059773842050 ),
 .UNSPECIFIED. ) ;
#12736 = AXIS2_PLACEMENT_3D ( 'NONE', #3345, #8181, #12962 ) ;
#12737 = FACE_BOUND ( 'NONE', #13423, .T. ) ;
#12738 = FACE_OUTER_BOUND ( 'NONE', #9067, .T. ) ;
#12739 = VECTOR ( 'NONE', #6823, 1000.000000000000000 ) ;
#12740 = DIRECTION ( 'NONE',  ( 1.000000000000000000, 0.000000000000000000, 0.000000000000000000 ) ) ;
#12741 = ADVANCED_FACE ( 'NONE', ( #14205 ), #3403, .F. ) ;
#12742 = CARTESIAN_POINT ( 'NONE',  ( -2.934533493136165738, 18.80010230636887414, -0.4000000000000101807 ) ) ;
#12743 = CARTESIAN_POINT ( 'NONE',  ( 14.00000000000004086, 64.51493994372674479, 15.00000000000104983 ) ) ;
#12744 = EDGE_CURVE ( 'NONE', #973, #9587, #12868, .T. ) ;
#12745 = ORIENTED_EDGE ( 'NONE', *, *, #15080, .T. ) ;
#12746 = DIRECTION ( 'NONE',  ( -0.000000000000000000, -0.000000000000000000, 1.000000000000000000 ) ) ;
#12747 = CARTESIAN_POINT ( 'NONE',  ( -200.8348121886614024, 140.6195990399117477, 9.578254705571838556 ) ) ;
#12748 = DIRECTION ( 'NONE',  ( 0.000000000000000000, 1.000000000000000000, 6.938893903907227145E-17 ) ) ;
#12749 = DIRECTION ( 'NONE',  ( 0.6130913241491352528, 0.7900120431063439863, -6.390853288715847897E-17 ) ) ;
#12750 = VERTEX_POINT ( 'NONE', #5852 ) ;
#12751 = VECTOR ( 'NONE', #14063, 1000.000000000000000 ) ;
#12752 = DIRECTION ( 'NONE',  ( 3.965082230804130220E-16, 1.090924371466202084E-47, 1.000000000000000000 ) ) ;
#12753 = ORIENTED_EDGE ( 'NONE', *, *, #8531, .F. ) ;
#12754 = ORIENTED_EDGE ( 'NONE', *, *, #11072, .T. ) ;
#12755 = FACE_OUTER_BOUND ( 'NONE', #11782, .T. ) ;
#12756 = DIRECTION ( 'NONE',  ( 0.000000000000000000, -0.000000000000000000, 1.000000000000000000 ) ) ;
#12757 = ADVANCED_FACE ( 'NONE', ( #10669 ), #4172, .F. ) ;
#12758 = CARTESIAN_POINT ( 'NONE',  ( 164.0000000000000568, 62.13993994372673768, 16.70000000000000995 ) ) ;
#12759 = CARTESIAN_POINT ( 'NONE',  ( -169.5864954465999972, 124.3918447529796509, 9.093140960474290324 ) ) ;
#12760 = CARTESIAN_POINT ( 'NONE',  ( -63.50000000000002842, 16.03993994372673981, -2.500000000000071498 ) ) ;
#12761 = DIRECTION ( 'NONE',  ( 0.000000000000000000, 0.000000000000000000, 1.000000000000000000 ) ) ;
#12762 = AXIS2_PLACEMENT_3D ( 'NONE', #9173, #7990, #12776 ) ;
#12763 = FACE_OUTER_BOUND ( 'NONE', #7918, .T. ) ;
#12764 = CARTESIAN_POINT ( 'NONE',  ( -64.00000000000002842, -178.8058001507315566, -17.69066787724516843 ) ) ;
#12765 = LINE ( 'NONE', #15594, #8942 ) ;
#12766 = EDGE_CURVE ( 'NONE', #3817, #10635, #7475, .T. ) ;
#12767 = LINE ( 'NONE', #10568, #15121 ) ;
#12768 = CARTESIAN_POINT ( 'NONE',  ( -223.3602385079212524, 147.0542838629705500, -2.257390888005822216 ) ) ;
#12769 = VERTEX_POINT ( 'NONE', #519 ) ;
#12770 = CARTESIAN_POINT ( 'NONE',  ( 172.5293059057019889, 61.25683321636181233, 10.00000000000000178 ) ) ;
#12771 = ORIENTED_EDGE ( 'NONE', *, *, #4196, .T. ) ;
#12772 = DIRECTION ( 'NONE',  ( 0.000000000000000000, 0.000000000000000000, 1.000000000000000000 ) ) ;
#12773 = DIRECTION ( 'NONE',  ( 1.000000000000000000, 0.000000000000000000, 0.000000000000000000 ) ) ;
#12774 = ORIENTED_EDGE ( 'NONE', *, *, #3635, .T. ) ;
#12775 = CARTESIAN_POINT ( 'NONE',  ( 71.96535645333923981, 38.79159067395544014, 10.00000000000000178 ) ) ;
#12776 = DIRECTION ( 'NONE',  ( 0.000000000000000000, -0.000000000000000000, -1.000000000000000000 ) ) ;
#12777 = DIRECTION ( 'NONE',  ( -0.000000000000000000, 1.000000000000000000, -0.000000000000000000 ) ) ;
#12778 = EDGE_LOOP ( 'NONE', ( #4980, #3998, #504, #11857 ) ) ;
#12779 = VERTEX_POINT ( 'NONE', #11436 ) ;
#12780 = EDGE_CURVE ( 'NONE', #15235, #2394, #13756, .T. ) ;
#12781 = CARTESIAN_POINT ( 'NONE',  ( 203.9349922441545857, 30.00251698353133989, -9.664403529890410738 ) ) ;
#12783 = EDGE_CURVE ( 'NONE', #15168, #10673, #13498, .T. ) ;
#12782 = EDGE_CURVE ( 'NONE', #7029, #4447, #7902, .T. ) ;
#12784 = DIRECTION ( 'NONE',  ( -1.000000000000000000, 0.000000000000000000, 0.000000000000000000 ) ) ;
#12785 = ORIENTED_EDGE ( 'NONE', *, *, #13444, .F. ) ;
#12786 = CARTESIAN_POINT ( 'NONE',  ( -34.79899788034579444, 48.72489408690345414, 5.000000000000000000 ) ) ;
#12787 = DIRECTION ( 'NONE',  ( -0.4873681696970814103, -0.8731965799097685110, -0.000000000000000000 ) ) ;
#12788 = EDGE_LOOP ( 'NONE', ( #12480, #2343, #1515, #6237 ) ) ;
#12789 = VERTEX_POINT ( 'NONE', #1870 ) ;
#12790 = FACE_OUTER_BOUND ( 'NONE', #7531, .T. ) ;
#12791 = DIRECTION ( 'NONE',  ( 0.000000000000000000, 0.000000000000000000, -1.000000000000000000 ) ) ;
#12792 = ORIENTED_EDGE ( 'NONE', *, *, #13104, .F. ) ;
#12793 = AXIS2_PLACEMENT_3D ( 'NONE', #9780, #354, #11201 ) ;
#12794 = CARTESIAN_POINT ( 'NONE',  ( 0.1306530452038150159, -5.952467836904141940, 5.690023276062422752 ) ) ;
#12795 = CARTESIAN_POINT ( 'NONE',  ( -63.50000000000002842, 15.03993994372673804, 37.07518420361041933 ) ) ;
#12796 = CIRCLE ( 'NONE', #10801, 1.499999999999999778 ) ;
#12797 = CARTESIAN_POINT ( 'NONE',  ( 175.9483885134608272, -178.8058001507315566, 52.19066787724494816 ) ) ;
#12798 = LINE ( 'NONE', #10218, #4436 ) ;
#12799 = DIRECTION ( 'NONE',  ( 0.000000000000000000, 0.000000000000000000, 1.000000000000000000 ) ) ;
#12800 = PRODUCT_DEFINITION_SHAPE ( 'NONE', 'NONE',  #6635 ) ;
#12801 = FACE_BOUND ( 'NONE', #4548, .T. ) ;
#12802 = AXIS2_PLACEMENT_3D ( 'NONE', #12553, #5546, #786 ) ;
#12803 = ORIENTED_EDGE ( 'NONE', *, *, #14066, .F. ) ;
#12804 = DIRECTION ( 'NONE',  ( 0.000000000000000000, 1.000000000000000000, 0.000000000000000000 ) ) ;
#12805 = AXIS2_PLACEMENT_3D ( 'NONE', #347, #2668, #7486 ) ;
#12806 = CARTESIAN_POINT ( 'NONE',  ( -202.0520865685784884, 146.2723300204251018, -0.4547266291960743168 ) ) ;
#12807 = CARTESIAN_POINT ( 'NONE',  ( 175.9483885134608272, 15.53993994372673981, 37.49999999999991473 ) ) ;
#12808 = EDGE_LOOP ( 'NONE', ( #4133, #10478, #8575, #3086, #15581, #6582 ) ) ;
#12809 = CARTESIAN_POINT ( 'NONE',  ( -216.0630845075784805, 143.0974466248333954, -4.642206099735013858 ) ) ;
#12810 = CARTESIAN_POINT ( 'NONE',  ( 202.4110361843541455, 29.59410989755560806, -6.585651355106874050 ) ) ;
#12811 = ADVANCED_FACE ( 'NONE', ( #1717 ), #5516, .T. ) ;
#12812 = VERTEX_POINT ( 'NONE', #602 ) ;
#12813 = CIRCLE ( 'NONE', #1218, 1.699999999999993072 ) ;
#12814 = CARTESIAN_POINT ( 'NONE',  ( -76.50000000000001421, 14.90076684276668040, -2.084916134869001958 ) ) ;
#12815 = CARTESIAN_POINT ( 'NONE',  ( -76.00000000000004263, 15.53993994372673804, 37.49999999999991473 ) ) ;
#12816 = AXIS2_PLACEMENT_3D ( 'NONE', #15271, #7009, #14021 ) ;
#12817 = PRODUCT_DEFINITION_FORMATION_WITH_SPECIFIED_SOURCE ( 'ANY', '', #5635, .NOT_KNOWN. ) ;
#12818 = FACE_BOUND ( 'NONE', #2467, .T. ) ;
#12819 = AXIS2_PLACEMENT_3D ( 'NONE', #7246, #1213, #100 ) ;
#12820 = EDGE_CURVE ( 'NONE', #6134, #9639, #12685, .T. ) ;
#12821 = VERTEX_POINT ( 'NONE', #5357 ) ;
#12822 = DIRECTION ( 'NONE',  ( -1.000000000000000000, 0.000000000000000000, 0.000000000000000000 ) ) ;
#12823 = VERTEX_POINT ( 'NONE', #10252 ) ;
#12824 = DIRECTION ( 'NONE',  ( 1.000000000000000000, 0.000000000000000000, 0.000000000000000000 ) ) ;
#12825 = CARTESIAN_POINT ( 'NONE',  ( -181.1823003367078115, 126.0769834546670296, 10.16010209732750624 ) ) ;
#12826 = CIRCLE ( 'NONE', #12335, 0.5000000000000004441 ) ;
#12827 = CARTESIAN_POINT ( 'NONE',  ( 169.5018791832601721, 101.0521538385604003, 5.000000000000000000 ) ) ;
#12828 = DIRECTION ( 'NONE',  ( -0.8204839007831782327, 0.5707893219124419160, -0.03171306586179808984 ) ) ;
#12829 = ORIENTED_EDGE ( 'NONE', *, *, #3894, .T. ) ;
#12830 = CARTESIAN_POINT ( 'NONE',  ( -35.99999999999995026, 62.13993994372673768, 15.00000000000139977 ) ) ;
#12831 = CIRCLE ( 'NONE', #15088, 3.500000000000003109 ) ;
#12832 = EDGE_LOOP ( 'NONE', ( #5738, #5155, #7584, #10987 ) ) ;
#12833 = ORIENTED_EDGE ( 'NONE', *, *, #1198, .F. ) ;
#12834 = CARTESIAN_POINT ( 'NONE',  ( -152.0432540882499666, 108.0562243547046535, 9.692725945294370149 ) ) ;
#12835 = DIRECTION ( 'NONE',  ( -0.000000000000000000, -0.000000000000000000, 1.000000000000000000 ) ) ;
#12836 = CARTESIAN_POINT ( 'NONE',  ( 175.9483885134608272, -179.3058001507315566, 84.88378295107887084 ) ) ;
#12837 = CARTESIAN_POINT ( 'NONE',  ( -167.9557412913654844, 127.3135968073034974, 4.793417203503699930 ) ) ;
#12838 = VECTOR ( 'NONE', #3992, 1000.000000000000000 ) ;
#12839 = EDGE_CURVE ( 'NONE', #3324, #13575, #9486, .T. ) ;
#12840 = CARTESIAN_POINT ( 'NONE',  ( -220.6535933262513822, 147.7382320429851177, -5.005762723283130100 ) ) ;
#12841 = VECTOR ( 'NONE', #5783, 1000.000000000000114 ) ;
#12842 = AXIS2_PLACEMENT_3D ( 'NONE', #7272, #2602, #57 ) ;
#12843 = DIRECTION ( 'NONE',  ( -0.4630766004634062072, -0.8863182623094566503, 0.000000000000000000 ) ) ;
#12844 = LINE ( 'NONE', #15127, #13687 ) ;
#12845 = DIRECTION ( 'NONE',  ( -0.000000000000000000, 0.000000000000000000, 1.000000000000000000 ) ) ;
#12846 = DIRECTION ( 'NONE',  ( 1.000000000000000000, 0.000000000000000000, 0.000000000000000000 ) ) ;
#12847 = AXIS2_PLACEMENT_3D ( 'NONE', #1037, #8247, #13023 ) ;
#12848 = DIRECTION ( 'NONE',  ( -0.000000000000000000, 1.000000000000000000, 0.000000000000000000 ) ) ;
#12849 = ORIENTED_EDGE ( 'NONE', *, *, #5310, .F. ) ;
#12850 = CIRCLE ( 'NONE', #12842, 5.000000000000004441 ) ;
#12851 = ORIENTED_EDGE ( 'NONE', *, *, #12184, .F. ) ;
#12852 = DIRECTION ( 'NONE',  ( 0.000000000000000000, 4.956352788505162775E-17, -1.000000000000000000 ) ) ;
#12853 = CIRCLE ( 'NONE', #7903, 0.5000000000000004441 ) ;
#12854 = CARTESIAN_POINT ( 'NONE',  ( 0.7145311798163258565, -9.237604307034018802, 2.775557561562891351E-14 ) ) ;
#12855 = CARTESIAN_POINT ( 'NONE',  ( -31.29899788034579800, 48.72489408690345414, 9.975000000000001421 ) ) ;
#12856 = DIRECTION ( 'NONE',  ( -0.000000000000000000, -0.000000000000000000, -1.000000000000000000 ) ) ;
#12857 = EDGE_CURVE ( 'NONE', #6660, #4287, #643, .T. ) ;
#12858 = AXIS2_PLACEMENT_3D ( 'NONE', #8959, #15007, #12128 ) ;
#12859 = DIRECTION ( 'NONE',  ( 0.000000000000000000, 1.486905836551548832E-16, -1.000000000000000000 ) ) ;
#12860 = ORIENTED_EDGE ( 'NONE', *, *, #11049, .F. ) ;
#12861 = VECTOR ( 'NONE', #3496, 1000.000000000000000 ) ;
#12862 = AXIS2_PLACEMENT_3D ( 'NONE', #7797, #11497, #4067 ) ;
#12863 = ITEM_DEFINED_TRANSFORMATION ( 'NONE', 'NONE', #10555,  #12337 ) ;
#12864 = VERTEX_POINT ( 'NONE', #7821 ) ;
#12865 = CARTESIAN_POINT ( 'NONE',  ( 209.6393851568315938, 47.95822392590527983, 0.3767681043515945238 ) ) ;
#12866 = DIRECTION ( 'NONE',  ( -1.000000000000000000, -1.669238443041287922E-16, 0.000000000000000000 ) ) ;
#12867 = ORIENTED_EDGE ( 'NONE', *, *, #2082, .F. ) ;
#12868 = LINE ( 'NONE', #3475, #6213 ) ;
#12869 = DIRECTION ( 'NONE',  ( 0.000000000000000000, -1.000000000000000000, -1.156482317317871478E-16 ) ) ;
#12870 = CYLINDRICAL_SURFACE ( 'NONE', #9077, 1.000000000000000888 ) ;
#12871 = VECTOR ( 'NONE', #13806, 1000.000000000000000 ) ;
#12872 = ORIENTED_EDGE ( 'NONE', *, *, #1908, .F. ) ;
#12873 = ORIENTED_EDGE ( 'NONE', *, *, #4489, .T. ) ;
#12874 = CARTESIAN_POINT ( 'NONE',  ( 190.0000000000000853, -178.6666270497714777, 53.18093594598651919 ) ) ;
#12875 = EDGE_CURVE ( 'NONE', #5311, #13177, #11503, .T. ) ;
#12876 = DIRECTION ( 'NONE',  ( 0.000000000000000000, 1.486905836551548832E-16, -1.000000000000000000 ) ) ;
#12877 = AXIS2_PLACEMENT_3D ( 'NONE', #6591, #15004, #15469 ) ;
#12878 = ORIENTED_EDGE ( 'NONE', *, *, #14885, .T. ) ;
#12879 = FACE_OUTER_BOUND ( 'NONE', #1533, .T. ) ;
#12880 = CYLINDRICAL_SURFACE ( 'NONE', #223, 8.000000000000028422 ) ;
#12881 = DIRECTION ( 'NONE',  ( 0.000000000000000000, 0.000000000000000000, 1.000000000000000000 ) ) ;
#12882 = PRODUCT_DEFINITION ( 'UNKNOWN', '', #188, #6482 ) ;
#12883 = DIRECTION ( 'NONE',  ( 0.000000000000000000, 0.000000000000000000, 1.000000000000000000 ) ) ;
#12884 = EDGE_CURVE ( 'NONE', #8326, #8197, #12609, .T. ) ;
#12885 = AXIS2_PLACEMENT_3D ( 'NONE', #14750, #9728, #3948 ) ;
#12886 = CYLINDRICAL_SURFACE ( 'NONE', #6311, 3.500000000000001332 ) ;
#12887 =( GEOMETRIC_REPRESENTATION_CONTEXT ( 3 ) GLOBAL_UNCERTAINTY_ASSIGNED_CONTEXT ( ( #574 ) ) GLOBAL_UNIT_ASSIGNED_CONTEXT ( ( #14890, #14737, #12374 ) ) REPRESENTATION_CONTEXT ( 'NONE', 'WORKASPACE' ) );
#12888 = ORIENTED_EDGE ( 'NONE', *, *, #9833, .T. ) ;
#12889 = DIRECTION ( 'NONE',  ( -0.000000000000000000, 1.000000000000000000, -0.000000000000000000 ) ) ;
#12890 = CARTESIAN_POINT ( 'NONE',  ( -207.9521514620915639, 147.4834172152791325, -2.963320117457100888 ) ) ;
#12891 = CARTESIAN_POINT ( 'NONE',  ( 13.88529453487718968, 40.04259805664093363, 10.00000000000000178 ) ) ;
#12892 = EDGE_LOOP ( 'NONE', ( #14909, #6185, #6916, #632 ) ) ;
#12893 = CARTESIAN_POINT ( 'NONE',  ( -181.9037801448002938, 118.7381910193847716, -0.5218507872395746761 ) ) ;
#12894 = CARTESIAN_POINT ( 'NONE',  ( 188.3076603040395582, 42.49356297222218615, -1.493920802967548367 ) ) ;
#12895 = ORIENTED_EDGE ( 'NONE', *, *, #11169, .T. ) ;
#12896 = CONICAL_SURFACE ( 'NONE', #15164, 4.499999999999950262, 0.7853981633974450594 ) ;
#12897 = EDGE_CURVE ( 'NONE', #1610, #15505, #6712, .T. ) ;
#12898 = DIRECTION ( 'NONE',  ( 0.000000000000000000, 1.156482317317871725E-16, -1.000000000000000000 ) ) ;
#12899 = CARTESIAN_POINT ( 'NONE',  ( 162.8297652159045015, 17.20175482153035063, -6.370175303308202253 ) ) ;
#12901 = ADVANCED_FACE ( 'NONE', ( #13792 ), #11594, .T. ) ;
#12900 = APPLICATION_CONTEXT ( 'automotive_design' ) ;
#12902 = AXIS2_PLACEMENT_3D ( 'NONE', #11601, #14975, #9083 ) ;
#12903 = DIRECTION ( 'NONE',  ( -0.000000000000000000, 1.000000000000000000, -0.000000000000000000 ) ) ;
#12904 = ORIENTED_EDGE ( 'NONE', *, *, #5758, .F. ) ;
#12905 = CARTESIAN_POINT ( 'NONE',  ( 0.000000000000000000, 0.000000000000000000, 0.000000000000000000 ) ) ;
#12906 = DIRECTION ( 'NONE',  ( 1.000000000000000000, 0.000000000000000000, 0.000000000000000000 ) ) ;
#12907 = ORIENTED_EDGE ( 'NONE', *, *, #3722, .F. ) ;
#12908 = DIRECTION ( 'NONE',  ( -0.000000000000000000, -0.000000000000000000, 1.000000000000000000 ) ) ;
#12909 = CARTESIAN_POINT ( 'NONE',  ( -197.4591130885309553, 135.0981391493542105, 10.16010209732750802 ) ) ;
#12910 = FACE_BOUND ( 'NONE', #14612, .T. ) ;
#12911 = DIRECTION ( 'NONE',  ( 0.8731965799097682890, -0.4873681696970819099, -0.000000000000000000 ) ) ;
#12912 = ORIENTED_EDGE ( 'NONE', *, *, #4815, .T. ) ;
#12913 = AXIS2_PLACEMENT_3D ( 'NONE', #10816, #3778, #8604 ) ;
#12914 = DIRECTION ( 'NONE',  ( 0.000000000000000000, 0.000000000000000000, -1.000000000000000000 ) ) ;
#12915 = EDGE_CURVE ( 'NONE', #3955, #4984, #10177, .T. ) ;
#12916 = ORIENTED_EDGE ( 'NONE', *, *, #9924, .F. ) ;
#12917 = ORIENTED_EDGE ( 'NONE', *, *, #10394, .T. ) ;
#12918 = CARTESIAN_POINT ( 'NONE',  ( 178.0000000000000853, -179.8058001507315566, 52.49999999999997868 ) ) ;
#12919 = DIRECTION ( 'NONE',  ( 0.4999999999999997224, 0.8660254037844387076, 0.000000000000000000 ) ) ;
#12920 = CARTESIAN_POINT ( 'NONE',  ( 114.0000000000000568, 64.53993994372673626, 15.00000000000035172 ) ) ;
#12921 = CARTESIAN_POINT ( 'NONE',  ( -173.1348595683955978, 118.0343934295742656, 8.028916588137546384 ) ) ;
#12922 = CARTESIAN_POINT ( 'NONE',  ( -221.1215437059437647, 151.0652570165180748, -4.807651471730975068 ) ) ;
#12923 = CARTESIAN_POINT ( 'NONE',  ( -216.7478739536621504, 154.8015167611612810, 3.747099613486799097 ) ) ;
#12924 = CARTESIAN_POINT ( 'NONE',  ( 175.9483885134608272, -179.3058001507315566, -29.88378295107906624 ) ) ;
#12925 = CYLINDRICAL_SURFACE ( 'NONE', #6002, 380.9270036976043343 ) ;
#12926 = DIRECTION ( 'NONE',  ( 0.7071067811864983899, 0.000000000000000000, 0.7071067811865966446 ) ) ;
#12927 = CARTESIAN_POINT ( 'NONE',  ( -85.27455057502459113, 65.19100426474074084, 10.00000000000000178 ) ) ;
#12928 = EDGE_CURVE ( 'NONE', #1071, #4381, #8138, .T. ) ;
#12929 = LINE ( 'NONE', #11991, #15413 ) ;
#12930 = ORIENTED_EDGE ( 'NONE', *, *, #4363, .F. ) ;
#12931 = ORIENTED_EDGE ( 'NONE', *, *, #13495, .T. ) ;
#12932 = CARTESIAN_POINT ( 'NONE',  ( 119.0806775638430253, 45.00321902537314145, 9.975000000000001421 ) ) ;
#12933 = CARTESIAN_POINT ( 'NONE',  ( -85.99999999999994316, 64.51493994372674479, 11.50000000000174438 ) ) ;
#12934 = VERTEX_POINT ( 'NONE', #2030 ) ;
#12935 = SURFACE_STYLE_USAGE ( .BOTH. , #14348 ) ;
#12936 = DIRECTION ( 'NONE',  ( -0.000000000000000000, 1.000000000000000000, -0.000000000000000000 ) ) ;
#12937 = PRODUCT ( 'hex bolt gradeab_iso_ISO 4014 - M10 x 45 x 26-N', 'hex bolt gradeab_iso_ISO 4014 - M10 x 45 x 26-N', '', ( #381 ) ) ;
#12938 = AXIS2_PLACEMENT_3D ( 'NONE', #755, #4314, #6941 ) ;
#12939 = VERTEX_POINT ( 'NONE', #15277 ) ;
#12940 = VERTEX_POINT ( 'NONE', #8998 ) ;
#12941 = AXIS2_PLACEMENT_3D ( 'NONE', #10645, #4636, #8368 ) ;
#12942 = CARTESIAN_POINT ( 'NONE',  ( 209.5531742284681798, 48.05466962632709027, -5.762314779011898480 ) ) ;
#12943 = CARTESIAN_POINT ( 'NONE',  ( 177.5000000000000853, -178.7362136002515172, 52.68580191161573367 ) ) ;
#12944 = ORIENTED_EDGE ( 'NONE', *, *, #14145, .F. ) ;
#12945 = DIRECTION ( 'NONE',  ( 0.000000000000000000, -1.000000000000000000, 0.000000000000000000 ) ) ;
#12946 = AXIS2_PLACEMENT_3D ( 'NONE', #2969, #11109, #7795 ) ;
#12947 = DIRECTION ( 'NONE',  ( 0.000000000000000000, 0.000000000000000000, -1.000000000000000000 ) ) ;
#12948 = DIRECTION ( 'NONE',  ( -0.000000000000000000, 1.000000000000000000, 0.000000000000000000 ) ) ;
#12949 = ORIENTED_EDGE ( 'NONE', *, *, #3825, .T. ) ;
#12950 = ORIENTED_EDGE ( 'NONE', *, *, #13462, .T. ) ;
#12951 = CARTESIAN_POINT ( 'NONE',  ( -35.99999999999995026, 59.53993994372674337, 15.00000000000139977 ) ) ;
#12952 = DIRECTION ( 'NONE',  ( -0.000000000000000000, 1.000000000000000000, -0.000000000000000000 ) ) ;
#12953 = ORIENTED_EDGE ( 'NONE', *, *, #4835, .F. ) ;
#12954 = CARTESIAN_POINT ( 'NONE',  ( -151.9073788345225466, 106.3957283150743081, 9.183240261263458493 ) ) ;
#12955 = DIRECTION ( 'NONE',  ( 0.000000000000000000, 0.000000000000000000, 1.000000000000000000 ) ) ;
#12956 = EDGE_CURVE ( 'NONE', #5373, #10184, #11434, .T. ) ;
#12957 = CIRCLE ( 'NONE', #10198, 8.000000000000028422 ) ;
#12958 = CARTESIAN_POINT ( 'NONE',  ( -76.00000000000001421, -178.8058001507315566, -17.19066787724516843 ) ) ;
#12959 = AXIS2_PLACEMENT_3D ( 'NONE', #12539, #1732, #10037 ) ;
#12960 = CARTESIAN_POINT ( 'NONE',  ( 178.0000000000000853, 15.03993994372673981, 10.05257423913146475 ) ) ;
#12961 = ORIENTED_EDGE ( 'NONE', *, *, #244, .F. ) ;
#12962 = DIRECTION ( 'NONE',  ( 0.000000000000000000, 0.000000000000000000, 1.000000000000000000 ) ) ;
#12963 = VECTOR ( 'NONE', #4638, 1000.000000000000000 ) ;
#12964 = EDGE_CURVE ( 'NONE', #15483, #7789, #4879, .T. ) ;
#12965 = DIRECTION ( 'NONE',  ( 1.000000000000000000, 0.000000000000000000, 0.000000000000000000 ) ) ;
#12966 =( BOUNDED_SURFACE ( )  B_SPLINE_SURFACE ( 3, 2, ( 
 ( #3476, #7046, #5854 ),
 ( #6738, #700, #3328 ),
 ( #10357, #9184, #15153 ),
 ( #14052, #8167, #8086 ),
 ( #867, #5699, #9723 ),
 ( #11058, #7362, #1176 ),
 ( #2612, #4737, #7130 ),
 ( #12157, #9644, #2449 ),
 ( #3559, #11932, #1409 ),
 ( #14440, #8314, #1335 ),
 ( #3636, #6008, #2376 ),
 ( #2295, #8469, #13097 ),
 ( #10912, #12231, #6244 ),
 ( #6094, #1105, #8616 ),
 ( #5924, #10832, #15534 ),
 ( #8398, #10749, #6174 ),
 ( #209, #10312, #68 ),
 ( #7209, #13251, #14593 ),
 ( #4907, #9561, #7282 ),
 ( #5057, #9882, #12079 ),
 ( #14672, #14363, #4823 ),
 ( #1258, #10986, #136 ),
 ( #14516, #13176, #3710 ),
 ( #8539, #12009, #13330 ),
 ( #9796, #2532, #4979 ),
 ( #3794, #13414, #7436 ),
 ( #11140, #4017, #13561 ),
 ( #11445, #2848, #8850 ),
 ( #3872, #1571, #10032 ),
 ( #369, #7672, #12462 ),
 ( #6408, #1806, #14819 ),
 ( #13641, #9961, #14902 ),
 ( #14977, #1651, #11216 ),
 ( #4097, #294, #5287 ),
 ( #6646, #611, #6488 ),
 ( #5134, #11285, #5210 ),
 ( #446, #10110, #13800 ),
 ( #10262, #14747, #3945 ),
 ( #10187, #3000, #8696 ),
 ( #8931, #5448, #2927 ),
 ( #2768, #4168, #12534 ),
 ( #13725, #7832, #12620 ),
 ( #13486, #7751, #1727 ),
 ( #2690, #8766, #6567 ),
 ( #11370, #7592, #529 ),
 ( #5366, #7509, #12387 ),
 ( #12305, #9006, #1490 ),
 ( #6328, #6792, #10573 ) ),
 .UNSPECIFIED., .F., .F., .T. ) 
 B_SPLINE_SURFACE_WITH_KNOTS ( ( 4, 2, 2, 2, 2, 2, 2, 2, 2, 2, 2, 2, 2, 2, 2, 2, 2, 2, 2, 2, 2, 2, 2, 4 ),
 ( 3, 3 ),
 ( 0.000000000000000000, 0.001056470869493305806, 0.001584706304239958709, 0.002112941738986611612, 0.003169412608479917418, 0.003697648043226570320, 0.004225883477973223223, 0.005282354347466529029, 0.005810589782213181932, 0.006338825216959834835, 0.007395296086453140641, 0.007923531521199792677, 0.008451766955946446447, 0.008980002390693100217, 0.009508237825439752253, 0.01056470869493305806, 0.01109294412967971183, 0.01162117956442636386, 0.01267765043391966967, 0.01373412130341297548, 0.01426235673815962751, 0.01479059217290628128, 0.01584706304239958535, 0.01690353391189289289 ),
 ( 0.000000000000000000, 1.000000000000000000 ),
 .UNSPECIFIED. ) 
 GEOMETRIC_REPRESENTATION_ITEM ( )  RATIONAL_B_SPLINE_SURFACE ( (
 ( 1.000000000000000000, 0.6642977373962596355, 1.000000000000000000),
 ( 1.000000000000000000, 0.6640838462638519735, 1.000000000000000000),
 ( 1.000000000000000000, 0.6642530361896505919, 1.000000000000000000),
 ( 1.000000000000000000, 0.6650420274440705937, 1.000000000000000000),
 ( 1.000000000000000000, 0.6653930490377342188, 1.000000000000000000),
 ( 1.000000000000000000, 0.6662696147822118053, 1.000000000000000000),
 ( 1.000000000000000000, 0.6667987513150220868, 1.000000000000000000),
 ( 1.000000000000000000, 0.6686259794347244600, 1.000000000000000000),
 ( 1.000000000000000000, 0.6701877536239834177, 1.000000000000000000),
 ( 1.000000000000000000, 0.6729075291465889119, 1.000000000000000000),
 ( 1.000000000000000000, 0.6738761219039702821, 1.000000000000000000),
 ( 1.000000000000000000, 0.6759369341149453758, 1.000000000000000000),
 ( 1.000000000000000000, 0.6770267051557863347, 1.000000000000000000),
 ( 1.000000000000000000, 0.6804085633467442662, 1.000000000000000000),
 ( 1.000000000000000000, 0.6828728915351610640, 1.000000000000000000),
 ( 1.000000000000000000, 0.6866515824972490023, 1.000000000000000000),
 ( 1.000000000000000000, 0.6879309149268769685, 1.000000000000000000),
 ( 1.000000000000000000, 0.6904804411488353333, 1.000000000000000000),
 ( 1.000000000000000000, 0.6917436029694029598, 1.000000000000000000),
 ( 1.000000000000000000, 0.6954928658986441192, 1.000000000000000000),
 ( 1.000000000000000000, 0.6979768248933013730, 1.000000000000000000),
 ( 1.000000000000000000, 0.7014000669802025190, 1.000000000000000000),
 ( 1.000000000000000000, 0.7024871511245815991, 1.000000000000000000),
 ( 1.000000000000000000, 0.7045189649009933053, 1.000000000000000000),
 ( 1.000000000000000000, 0.7054698226116191684, 1.000000000000000000),
 ( 1.000000000000000000, 0.7072451538296151696, 1.000000000000000000),
 ( 1.000000000000000000, 0.7080696632615188779, 1.000000000000000000),
 ( 1.000000000000000000, 0.7095909328304439434, 1.000000000000000000),
 ( 1.000000000000000000, 0.7102769625305951351, 1.000000000000000000),
 ( 1.000000000000000000, 0.7120402354171648796, 1.000000000000000000),
 ( 1.000000000000000000, 0.7128600990435562945, 1.000000000000000000),
 ( 1.000000000000000000, 0.7136629434598023014, 1.000000000000000000),
 ( 1.000000000000000000, 0.7138590768182416779, 1.000000000000000000),
 ( 1.000000000000000000, 0.7141136962395474574, 1.000000000000000000),
 ( 1.000000000000000000, 0.7141632686186834000, 1.000000000000000000),
 ( 1.000000000000000000, 0.7141258579405006524, 1.000000000000000000),
 ( 1.000000000000000000, 0.7138566471735118268, 1.000000000000000000),
 ( 1.000000000000000000, 0.7130110457638262345, 1.000000000000000000),
 ( 1.000000000000000000, 0.7124421886026640616, 1.000000000000000000),
 ( 1.000000000000000000, 0.7115151177449636766, 1.000000000000000000),
 ( 1.000000000000000000, 0.7111938932540499136, 1.000000000000000000),
 ( 1.000000000000000000, 0.7105477981655051734, 1.000000000000000000),
 ( 1.000000000000000000, 0.7102218485250791913, 1.000000000000000000),
 ( 1.000000000000000000, 0.7092850706994120458, 1.000000000000000000),
 ( 1.000000000000000000, 0.7087083600013776019, 1.000000000000000000),
 ( 1.000000000000000000, 0.7077862628354428809, 1.000000000000000000),
 ( 1.000000000000000000, 0.7074374214232334035, 1.000000000000000000),
 ( 1.000000000000000000, 0.7072571230115936025, 1.000000000000000000) ) ) 
 REPRESENTATION_ITEM ( '' )  SURFACE ( )  );
#12967 = CARTESIAN_POINT ( 'NONE',  ( 170.2911098586863545, 111.9959133412127272, 0.000000000000000000 ) ) ;
#12968 = VERTEX_POINT ( 'NONE', #1944 ) ;
#12969 = CARTESIAN_POINT ( 'NONE',  ( -222.0824530901772675, 149.3436370173336059, -5.265047855996057180 ) ) ;
#12970 = CARTESIAN_POINT ( 'NONE',  ( 201.2368453335255936, 49.57344380111126725, -8.378533376203868954 ) ) ;
#12971 = ORIENTED_EDGE ( 'NONE', *, *, #8548, .F. ) ;
#12972 = CARTESIAN_POINT ( 'NONE',  ( -76.00000000000004263, 14.97035339324670744, 37.58005016923963382 ) ) ;
#12973 = CARTESIAN_POINT ( 'NONE',  ( 215.1062858801516882, 55.86394065090267702, 18.00000000000000355 ) ) ;
#12974 = CARTESIAN_POINT ( 'NONE',  ( -150.5342426605305945, 106.7706832906523999, -4.718200141660423341 ) ) ;
#12975 = AXIS2_PLACEMENT_3D ( 'NONE', #9578, #8329, #4520 ) ;
#12976 = ORIENTED_EDGE ( 'NONE', *, *, #13378, .T. ) ;
#12977 = SHAPE_REPRESENTATION_RELATIONSHIP ( 'NONE' , 'NONE' ,  #12546, #6616 ) ;
#12978 = CARTESIAN_POINT ( 'NONE',  ( 0.4969600502617326776, 4.995646404165254850, -7.347286611336954820 ) ) ;
#12979 = CARTESIAN_POINT ( 'NONE',  ( 201.3139613293953971, 49.56665511821758230, -6.809528532989353344 ) ) ;
#12980 = VERTEX_POINT ( 'NONE', #3071 ) ;
#12981 = DIRECTION ( 'NONE',  ( 1.000000000000000000, 2.751328491981765035E-32, -3.965082230804130220E-16 ) ) ;
#12982 = ADVANCED_FACE ( 'NONE', ( #6783 ), #14260, .F. ) ;
#12983 = CARTESIAN_POINT ( 'NONE',  ( -205.9652191273047777, 131.2378527988410326, 1.515400478619091329 ) ) ;
#12985 = ADVANCED_FACE ( 'NONE', ( #5902 ), #12683, .T. ) ;
#12984 = CARTESIAN_POINT ( 'NONE',  ( -150.4086188282879277, 107.2728346664360259, 9.719846845941791713 ) ) ;
#12986 = LINE ( 'NONE', #2177, #14603 ) ;
#12987 = DIRECTION ( 'NONE',  ( 1.000000000000000000, 0.000000000000000000, 0.000000000000000000 ) ) ;
#12988 = VECTOR ( 'NONE', #4035, 999.9999999999998863 ) ;
#12989 = ORIENTED_EDGE ( 'NONE', *, *, #5482, .T. ) ;
#12990 = ORIENTED_EDGE ( 'NONE', *, *, #2736, .F. ) ;
#12991 = DIRECTION ( 'NONE',  ( -0.000000000000000000, 1.000000000000000000, 6.938893903907227145E-17 ) ) ;
#12992 = DIRECTION ( 'NONE',  ( 0.000000000000000000, 0.000000000000000000, -1.000000000000000000 ) ) ;
#12993 = CARTESIAN_POINT ( 'NONE',  ( 184.0000000000000568, -181.3058001507315566, -41.45141194869120227 ) ) ;
#12994 = CARTESIAN_POINT ( 'NONE',  ( -224.1161033238799121, 145.7000333943786927, -3.784926783786191518 ) ) ;
#12995 = CARTESIAN_POINT ( 'NONE',  ( -223.2420850427828327, 142.7740955428692757, 6.010832199141798782 ) ) ;
#12996 = AXIS2_PLACEMENT_3D ( 'NONE', #5437, #15126, #11359 ) ;
#12997 = DIRECTION ( 'NONE',  ( -0.000000000000000000, -0.000000000000000000, 1.000000000000000000 ) ) ;
#12998 = DIRECTION ( 'NONE',  ( 0.000000000000000000, 0.000000000000000000, -1.000000000000000000 ) ) ;
#12999 = DIRECTION ( 'NONE',  ( 3.965082230804130220E-16, 1.486905836551548832E-16, -1.000000000000000000 ) ) ;
#13000 = CARTESIAN_POINT ( 'NONE',  ( 64.00000000000005684, 62.13993994372673768, 15.00000000000070166 ) ) ;
#13001 = CYLINDRICAL_SURFACE ( 'NONE', #2310, 0.4999999999999996114 ) ;
#13002 = VERTEX_POINT ( 'NONE', #1229 ) ;
#13003 = CARTESIAN_POINT ( 'NONE',  ( -34.79899788034579444, 48.72489408690345414, 10.00000000000000178 ) ) ;
#13004 = ORIENTED_EDGE ( 'NONE', *, *, #15132, .F. ) ;
#13005 = FACE_OUTER_BOUND ( 'NONE', #11274, .T. ) ;
#13006 = DIRECTION ( 'NONE',  ( 0.000000000000000000, 0.000000000000000000, 1.000000000000000000 ) ) ;
#13007 = CARTESIAN_POINT ( 'NONE',  ( 6.800000000000000711, 6.123233995736767268E-16, -5.000000000000000000 ) ) ;
#13008 = DIRECTION ( 'NONE',  ( 0.000000000000000000, 0.000000000000000000, 1.000000000000000000 ) ) ;
#13009 = CARTESIAN_POINT ( 'NONE',  ( 177.5000000000000853, -179.8058001507315566, 64.88378295107887084 ) ) ;
#13010 = AXIS2_PLACEMENT_3D ( 'NONE', #12663, #3277, #4374 ) ;
#13011 = ORIENTED_EDGE ( 'NONE', *, *, #567, .F. ) ;
#13012 = EDGE_CURVE ( 'NONE', #8751, #207, #5888, .T. ) ;
#13013 = VERTEX_POINT ( 'NONE', #4634 ) ;
#13014 = CARTESIAN_POINT ( 'NONE',  ( 202.5558682508970492, 29.63341987102701580, -9.723657537314917221 ) ) ;
#13015 = DIRECTION ( 'NONE',  ( 1.000000000000000000, 0.000000000000000000, 0.000000000000000000 ) ) ;
#13016 = ORIENTED_EDGE ( 'NONE', *, *, #7680, .T. ) ;
#13017 = CARTESIAN_POINT ( 'NONE',  ( 177.5000000000000853, 19.53993994372674337, 9.999999999999998224 ) ) ;
#13018 = VERTEX_POINT ( 'NONE', #3683 ) ;
#13019 = EDGE_LOOP ( 'NONE', ( #13004, #2048 ) ) ;
#13020 = DIRECTION ( 'NONE',  ( 0.000000000000000000, 0.000000000000000000, 1.000000000000000000 ) ) ;
#13021 = CARTESIAN_POINT ( 'NONE',  ( -139.4318739252458670, 92.47118091487817537, 5.000000000000000000 ) ) ;
#13022 = VERTEX_POINT ( 'NONE', #41 ) ;
#13023 = DIRECTION ( 'NONE',  ( 1.000000000000000000, 0.000000000000000000, 0.000000000000000000 ) ) ;
#13024 = AXIS2_PLACEMENT_3D ( 'NONE', #1396, #6234, #197 ) ;
#13025 = CARTESIAN_POINT ( 'NONE',  ( -156.6477983077465410, 110.1970436846185066, 0.000000000000000000 ) ) ;
#13026 = ORIENTED_EDGE ( 'NONE', *, *, #11468, .T. ) ;
#13027 = CARTESIAN_POINT ( 'NONE',  ( 122.5806775638430253, 45.00321902537314145, 5.000000000000000000 ) ) ;
#13028 = EDGE_CURVE ( 'NONE', #3064, #1731, #13715, .T. ) ;
#13029 = FACE_OUTER_BOUND ( 'NONE', #1106, .T. ) ;
#13030 = CIRCLE ( 'NONE', #15048, 3.525000000000000355 ) ;
#13031 = LINE ( 'NONE', #7065, #5309 ) ;
#13032 = CARTESIAN_POINT ( 'NONE',  ( 184.0000000000000568, 15.53993994372673626, 45.99999999999998579 ) ) ;
#13033 = ORIENTED_EDGE ( 'NONE', *, *, #1479, .T. ) ;
#13034 = CARTESIAN_POINT ( 'NONE',  ( -188.3338018137096128, 131.5603057966125675, -5.230826428279604201 ) ) ;
#13035 = CARTESIAN_POINT ( 'NONE',  ( 194.7786688470199010, 47.83282381504752578, -5.005399988216014506 ) ) ;
#13036 = AXIS2_PLACEMENT_3D ( 'NONE', #1084, #1159, #5988 ) ;
#13037 = EDGE_LOOP ( 'NONE', ( #551, #8735, #12643, #14605 ) ) ;
#13038 = CARTESIAN_POINT ( 'NONE',  ( 224.0000000000000853, 56.53993994372675047, 25.00000000000000000 ) ) ;
#13039 = CARTESIAN_POINT ( 'NONE',  ( -76.50000000000004263, 15.03993994372673804, 24.94742576086838781 ) ) ;
#13040 = CARTESIAN_POINT ( 'NONE',  ( 190.0000000000000568, -179.8058001507315566, -17.19066787724516843 ) ) ;
#13041 = EDGE_CURVE ( 'NONE', #10036, #12077, #4712, .T. ) ;
#13042 = CIRCLE ( 'NONE', #8294, 0.5000000000000004441 ) ;
#13043 = ORIENTED_EDGE ( 'NONE', *, *, #4535, .T. ) ;
#13044 = AXIS2_PLACEMENT_3D ( 'NONE', #15112, #10318, #2977 ) ;
#13045 = PRESENTATION_STYLE_ASSIGNMENT (( #1207 ) ) ;
#13046 = CARTESIAN_POINT ( 'NONE',  ( 191.3844089520862894, 42.02011290432638901, -3.056456915890917170 ) ) ;
#13047 = ORIENTED_EDGE ( 'NONE', *, *, #12505, .F. ) ;
#13048 = CARTESIAN_POINT ( 'NONE',  ( -223.5674327266374917, 142.0998017908669624, 1.142491232282270008 ) ) ;
#13049 = CARTESIAN_POINT ( 'NONE',  ( -225.7548303624725179, 142.7639966680278576, 3.410453015226076801 ) ) ;
#13050 = CARTESIAN_POINT ( 'NONE',  ( -76.00000000000004263, -178.9449732516916072, 64.32815825124538378 ) ) ;
#13051 = CARTESIAN_POINT ( 'NONE',  ( 0.4969600502617518845, 8.860760056385744932, 0.6527133886630305248 ) ) ;
#13052 = PRODUCT_DEFINITION_SHAPE ( 'NONE', 'NONE',  #15625 ) ;
#13053 = CARTESIAN_POINT ( 'NONE',  ( 193.1265229109121435, 35.50728864820005981, -5.680987958736793075 ) ) ;
#13054 = CIRCLE ( 'NONE', #5009, 1.000000000000000444 ) ;
#13055 = VERTEX_POINT ( 'NONE', #7019 ) ;
#13056 = ORIENTED_EDGE ( 'NONE', *, *, #10337, .F. ) ;
#13057 = CARTESIAN_POINT ( 'NONE',  ( -184.9746689684865260, 119.2870100535896682, 2.431555724346862846 ) ) ;
#13058 = PLANE ( 'NONE',  #8333 ) ;
#13059 =( GEOMETRIC_REPRESENTATION_CONTEXT ( 3 ) GLOBAL_UNCERTAINTY_ASSIGNED_CONTEXT ( ( #5825 ) ) GLOBAL_UNIT_ASSIGNED_CONTEXT ( ( #13653, #8706, #1423 ) ) REPRESENTATION_CONTEXT ( 'NONE', 'WORKASPACE' ) );
#13060 = EDGE_CURVE ( 'NONE', #1178, #12789, #11827, .T. ) ;
#13061 = CIRCLE ( 'NONE', #6276, 1.000000000000000888 ) ;
#13062 = DIRECTION ( 'NONE',  ( 1.000000000000000000, -0.000000000000000000, -0.000000000000000000 ) ) ;
#13063 = CARTESIAN_POINT ( 'NONE',  ( -130.9946291778373961, 96.97121815129470690, 5.000000000000000000 ) ) ;
#13064 = CARTESIAN_POINT ( 'NONE',  ( -223.1092991286456595, 142.9943895293494052, -1.544005151573194068 ) ) ;
#13065 = ADVANCED_FACE ( 'NONE', ( #13556 ), #1645, .F. ) ;
#13066 = EDGE_CURVE ( 'NONE', #3832, #10070, #7661, .T. ) ;
#13067 = CARTESIAN_POINT ( 'NONE',  ( -218.6461639067876206, 151.4790071514009639, 9.088489419225989963 ) ) ;
#13068 = LINE ( 'NONE', #3684, #5901 ) ;
#13069 = AXIS2_PLACEMENT_3D ( 'NONE', #613, #12622, #12772 ) ;
#13070 = ADVANCED_FACE ( 'NONE', ( #363 ), #5049, .F. ) ;
#13071 = DIRECTION ( 'NONE',  ( -1.000000000000000000, 0.000000000000000000, 0.000000000000000000 ) ) ;
#13072 = CARTESIAN_POINT ( 'NONE',  ( 0.000000000000000000, 0.000000000000000000, 0.000000000000000000 ) ) ;
#13073 = CIRCLE ( 'NONE', #10323, 1.500000000000001332 ) ;
#13074 = CARTESIAN_POINT ( 'NONE',  ( -193.7200834347810599, 142.0619459586758921, 2.500000000000000000 ) ) ;
#13075 = CARTESIAN_POINT ( 'NONE',  ( 0.2456200930618588907, -1.587713240271461546, 2.750000000000000000 ) ) ;
#13076 = DIRECTION ( 'NONE',  ( 0.000000000000000000, 0.9902680687415712502, 0.1391731009600584990 ) ) ;
#13077 = ORIENTED_EDGE ( 'NONE', *, *, #5171, .T. ) ;
#13078 =( NAMED_UNIT ( * ) PLANE_ANGLE_UNIT ( ) SI_UNIT ( $, .RADIAN. ) );
#13079 = VERTEX_POINT ( 'NONE', #12298 ) ;
#13080 = FACE_OUTER_BOUND ( 'NONE', #6241, .T. ) ;
#13081 =( LENGTH_UNIT ( ) NAMED_UNIT ( * ) SI_UNIT ( .MILLI., .METRE. ) );
#13082 = AXIS2_PLACEMENT_3D ( 'NONE', #2324, #3658, #1199 ) ;
#13083 = DIRECTION ( 'NONE',  ( 0.000000000000000000, 1.000000000000000000, 6.938893903907227145E-17 ) ) ;
#13084 = CARTESIAN_POINT ( 'NONE',  ( 183.0404880503516267, 40.86394065090267702, 5.000000000000000000 ) ) ;
#13085 = EDGE_CURVE ( 'NONE', #13090, #7984, #9953, .T. ) ;
#13086 = EDGE_CURVE ( 'NONE', #4984, #10665, #7745, .T. ) ;
#13087 = ORIENTED_EDGE ( 'NONE', *, *, #13202, .T. ) ;
#13088 = CIRCLE ( 'NONE', #3029, 1.000000000000000888 ) ;
#13089 = AXIS2_PLACEMENT_3D ( 'NONE', #11320, #10453, #1992 ) ;
#13090 = VERTEX_POINT ( 'NONE', #437 ) ;
#13091 = EDGE_CURVE ( 'NONE', #13177, #2407, #9877, .T. ) ;
#13092 = CARTESIAN_POINT ( 'NONE',  ( 202.8882743124338504, 32.81631024066724933, -8.087096619718394663 ) ) ;
#13093 = CARTESIAN_POINT ( 'NONE',  ( 0.3157512944565075141, -3.097794232830054728, 8.000000000000008882 ) ) ;
#13094 = VERTEX_POINT ( 'NONE', #6403 ) ;
#13096 = AXIS2_PLACEMENT_3D ( 'NONE', #10061, #5401, #13675 ) ;
#13095 = FACE_OUTER_BOUND ( 'NONE', #4579, .T. ) ;
#13097 = CARTESIAN_POINT ( 'NONE',  ( -224.1564255670275827, 145.6277897662952228, 5.545703538890369266 ) ) ;
#13098 = ORIENTED_EDGE ( 'NONE', *, *, #14788, .F. ) ;
#13099 = ORIENTED_EDGE ( 'NONE', *, *, #2285, .T. ) ;
#13100 = CARTESIAN_POINT ( 'NONE',  ( -218.1600191662880661, 152.2676192875508718, 2.431557144026069928 ) ) ;
#13101 = DIRECTION ( 'NONE',  ( 5.518327896226369609E-17, 0.9902680687415712502, 0.1391731009600584990 ) ) ;
#13102 = ADVANCED_FACE ( 'NONE', ( #11361 ), #12382, .F. ) ;
#13103 = EDGE_LOOP ( 'NONE', ( #15554, #14915, #12463, #8308 ) ) ;
#13104 = EDGE_CURVE ( 'NONE', #7691, #13181, #9251, .T. ) ;
#13105 = DIRECTION ( 'NONE',  ( 0.000000000000000000, 0.000000000000000000, 1.000000000000000000 ) ) ;
#13106 = PLANE ( 'NONE',  #2802 ) ;
#13107 = AXIS2_PLACEMENT_3D ( 'NONE', #2065, #1983, #3254 ) ;
#13108 = AXIS2_PLACEMENT_3D ( 'NONE', #13142, #2344, #5976 ) ;
#13109 = LINE ( 'NONE', #2385, #15176 ) ;
#13110 = EDGE_LOOP ( 'NONE', ( #6572, #4116, #2444, #389 ) ) ;
#13111 = DIRECTION ( 'NONE',  ( 1.000000000000000000, -0.000000000000000000, -0.000000000000000000 ) ) ;
#13112 = CIRCLE ( 'NONE', #1265, 0.5000000000000004441 ) ;
#13113 = VERTEX_POINT ( 'NONE', #6321 ) ;
#13114 = CARTESIAN_POINT ( 'NONE',  ( 177.5000000000000853, 16.03993994372673981, 10.05257423913146475 ) ) ;
#13115 = AXIS2_PLACEMENT_3D ( 'NONE', #7490, #12283, #12518 ) ;
#13116 = CARTESIAN_POINT ( 'NONE',  ( -214.8715905313398480, 153.8675021612092451, 2.500000000000000000 ) ) ;
#13117 = EDGE_CURVE ( 'NONE', #5937, #12099, #14193, .T. ) ;
#13118 = LINE ( 'NONE', #14152, #5026 ) ;
#13119 = ORIENTED_EDGE ( 'NONE', *, *, #1880, .T. ) ;
#13120 = CARTESIAN_POINT ( 'NONE',  ( -193.9023367725753815, 141.7188637290702502, -0.4547266291960752049 ) ) ;
#13121 = CARTESIAN_POINT ( 'NONE',  ( 207.3822464892701305, 31.45897796630539744, -3.508361229271337312 ) ) ;
#13122 = VERTEX_POINT ( 'NONE', #1800 ) ;
#13123 = LINE ( 'NONE', #2560, #15605 ) ;
#13124 = CYLINDRICAL_SURFACE ( 'NONE', #15509, 0.4999999999999996114 ) ;
#13125 = DIRECTION ( 'NONE',  ( 0.000000000000000000, 1.734723475976805517E-15, 1.000000000000000000 ) ) ;
#13126 = AXIS2_PLACEMENT_3D ( 'NONE', #9110, #8090, #12876 ) ;
#13127 = VECTOR ( 'NONE', #1559, 999.9999999999998863 ) ;
#13128 = ORIENTED_EDGE ( 'NONE', *, *, #3338, .T. ) ;
#13129 = DIRECTION ( 'NONE',  ( 0.000000000000000000, 0.000000000000000000, 1.000000000000000000 ) ) ;
#13130 = CARTESIAN_POINT ( 'NONE',  ( 207.1164837741930569, 35.57719129110033407, -1.806778302941847159 ) ) ;
#13131 = ORIENTED_EDGE ( 'NONE', *, *, #60, .T. ) ;
#13132 = CARTESIAN_POINT ( 'NONE',  ( 195.1062858801516597, 40.86394065090267702, 5.000000000000000000 ) ) ;
#13133 = CARTESIAN_POINT ( 'NONE',  ( -76.00000000000001421, -178.9449732516916072, -29.32815825124561471 ) ) ;
#13134 = CARTESIAN_POINT ( 'NONE',  ( -201.1640730962011219, 128.1953734590158263, 3.478895870929496148 ) ) ;
#13135 = CARTESIAN_POINT ( 'NONE',  ( 6.399999999999999467, -4.618802153516981868, 8.000000000000007105 ) ) ;
#13136 = FACE_OUTER_BOUND ( 'NONE', #9793, .T. ) ;
#13137 = CARTESIAN_POINT ( 'NONE',  ( -196.0016709267559349, 137.8086561579936813, 9.578254705571842109 ) ) ;
#13139 = DIRECTION ( 'NONE',  ( -0.000000000000000000, -1.000000000000000000, -0.000000000000000000 ) ) ;
#13138 = AXIS2_PLACEMENT_3D ( 'NONE', #9342, #3333, #8171 ) ;
#13140 = VERTEX_POINT ( 'NONE', #5600 ) ;
#13141 = ORIENTED_EDGE ( 'NONE', *, *, #9952, .F. ) ;
#13142 = CARTESIAN_POINT ( 'NONE',  ( 184.0000000000000568, -179.3058001507315566, -41.45141194869120227 ) ) ;
#13143 = FACE_BOUND ( 'NONE', #10167, .T. ) ;
#13144 = DIRECTION ( 'NONE',  ( 0.000000000000000000, -4.956352788505162775E-17, 1.000000000000000000 ) ) ;
#13145 = DIRECTION ( 'NONE',  ( 1.000000000000000000, 0.000000000000000000, 0.000000000000000000 ) ) ;
#13146 = CARTESIAN_POINT ( 'NONE',  ( -224.3577192345715048, 145.2671405631149355, 0.1302923618042369780 ) ) ;
#13147 = DIRECTION ( 'NONE',  ( -1.000000000000000000, 0.000000000000000000, 0.000000000000000000 ) ) ;
#13148 = CARTESIAN_POINT ( 'NONE',  ( 0.06730325657896167602, -1.557442666625575178, -7.999999999999979572 ) ) ;
#13149 = AXIS2_PLACEMENT_3D ( 'NONE', #1387, #9704, #6076 ) ;
#13150 = EDGE_CURVE ( 'NONE', #4389, #9280, #1945, .T. ) ;
#13151 = CARTESIAN_POINT ( 'NONE',  ( 122.5806775638430253, 45.00321902537314145, 10.00000000000000178 ) ) ;
#13152 = CARTESIAN_POINT ( 'NONE',  ( -187.9132138465967898, 138.8208849330412988, 2.500000000000000000 ) ) ;
#13153 = DIRECTION ( 'NONE',  ( 1.000000000000000000, 2.751328491981765035E-32, -3.965082230804130220E-16 ) ) ;
#13154 = CARTESIAN_POINT ( 'NONE',  ( -110.0000000000000426, 56.53993994372675047, 13.00000000000000178 ) ) ;
#13155 = ORIENTED_EDGE ( 'NONE', *, *, #8002, .T. ) ;
#13156 = ADVANCED_FACE ( 'NONE', ( #12763 ), #7975, .T. ) ;
#13157 =( LENGTH_UNIT ( ) NAMED_UNIT ( * ) SI_UNIT ( .MILLI., .METRE. ) );
#13158 = ORIENTED_EDGE ( 'NONE', *, *, #8099, .T. ) ;
#13159 = CARTESIAN_POINT ( 'NONE',  ( -34.79899788034579444, 48.72489408690345414, 10.00000000000000178 ) ) ;
#13160 = DIRECTION ( 'NONE',  ( 0.000000000000000000, 0.1391731009600626345, 0.9902680687415706950 ) ) ;
#13161 = CYLINDRICAL_SURFACE ( 'NONE', #15425, 3.500000000000003109 ) ;
#13162 = DIRECTION ( 'NONE',  ( -0.000000000000000000, 1.000000000000000000, -0.000000000000000000 ) ) ;
#13163 = CARTESIAN_POINT ( 'NONE',  ( 0.02377086945486034386, 0.5410735902665446684, 2.750000000000001332 ) ) ;
#13165 = AXIS2_PLACEMENT_3D ( 'NONE', #9630, #7350, #3623 ) ;
#13164 = CIRCLE ( 'NONE', #7644, 1.699999999999998401 ) ;
#13166 = FACE_OUTER_BOUND ( 'NONE', #3657, .T. ) ;
#13167 = CARTESIAN_POINT ( 'NONE',  ( -179.9267697467775520, 134.3633106217456543, 2.500000000000000000 ) ) ;
#13168 = EDGE_LOOP ( 'NONE', ( #4819, #12420, #4424, #14656 ) ) ;
#13169 = EDGE_LOOP ( 'NONE', ( #3065, #9665 ) ) ;
#13170 = CARTESIAN_POINT ( 'NONE',  ( 207.1750190499664370, 35.67744599754978907, -6.373597270514506974 ) ) ;
#13171 = DIRECTION ( 'NONE',  ( -1.000000000000000000, 0.000000000000000000, 0.000000000000000000 ) ) ;
#13172 = ORIENTED_EDGE ( 'NONE', *, *, #6516, .T. ) ;
#13173 = ADVANCED_FACE ( 'NONE', ( #13793, #8055 ), #3305, .T. ) ;
#13174 = EDGE_CURVE ( 'NONE', #8543, #4053, #12844, .T. ) ;
#13175 = ADVANCED_FACE ( 'NONE', ( #9231 ), #2031, .T. ) ;
#13176 = CARTESIAN_POINT ( 'NONE',  ( -222.9033204732309343, 147.8729242461827198, 9.743095389425892705 ) ) ;
#13177 = VERTEX_POINT ( 'NONE', #4320 ) ;
#13178 = ORIENTED_EDGE ( 'NONE', *, *, #5178, .T. ) ;
#13179 = DIRECTION ( 'NONE',  ( 1.000000000000000000, 0.000000000000000000, 0.000000000000000000 ) ) ;
#13180 = LINE ( 'NONE', #4663, #5588 ) ;
#13181 = VERTEX_POINT ( 'NONE', #5747 ) ;
#13182 = DIRECTION ( 'NONE',  ( -1.000000000000000000, 0.000000000000000000, 0.000000000000000000 ) ) ;
#13183 = DIRECTION ( 'NONE',  ( 0.4873681696970819655, 0.8731965799097684000, 0.000000000000000000 ) ) ;
#13184 = EDGE_CURVE ( 'NONE', #2617, #2533, #14697, .T. ) ;
#13185 = ORIENTED_EDGE ( 'NONE', *, *, #7671, .F. ) ;
#13186 = AXIS2_PLACEMENT_3D ( 'NONE', #5494, #9207, #15252 ) ;
#13187 = ORIENTED_EDGE ( 'NONE', *, *, #14470, .F. ) ;
#13188 = FACE_OUTER_BOUND ( 'NONE', #14531, .T. ) ;
#13189 = FACE_OUTER_BOUND ( 'NONE', #1375, .T. ) ;
#13190 = DIRECTION ( 'NONE',  ( -0.9741547192086867923, 0.2258817899775114602, 0.000000000000000000 ) ) ;
#13191 = VERTEX_POINT ( 'NONE', #4238 ) ;
#13192 = ORIENTED_EDGE ( 'NONE', *, *, #13104, .T. ) ;
#13193 = CARTESIAN_POINT ( 'NONE',  ( -189.8662655649658859, 135.3588663075204579, -4.640918829492423292 ) ) ;
#13194 = CARTESIAN_POINT ( 'NONE',  ( 208.7972876766878016, 42.12791357830437988, -6.002605234521809052 ) ) ;
#13195 = AXIS2_PLACEMENT_3D ( 'NONE', #8517, #9620, #1231 ) ;
#13196 = ORIENTED_EDGE ( 'NONE', *, *, #14332, .T. ) ;
#13197 = AXIS2_PLACEMENT_3D ( 'NONE', #2204, #15372, #5915 ) ;
#13198 = CARTESIAN_POINT ( 'NONE',  ( 175.9483885134608272, 15.53993994372673981, -2.500000000000070610 ) ) ;
#13199 = DIRECTION ( 'NONE',  ( 1.000000000000000000, 0.000000000000000000, 0.000000000000000000 ) ) ;
#13200 = CARTESIAN_POINT ( 'NONE',  ( -150.4086188282879277, 107.2728346664360259, -5.000000000000000000 ) ) ;
#13201 = EDGE_CURVE ( 'NONE', #4775, #7275, #2359, .T. ) ;
#13202 = EDGE_CURVE ( 'NONE', #3561, #4430, #1334, .T. ) ;
#13203 = VERTEX_POINT ( 'NONE', #9078 ) ;
#13204 = EDGE_CURVE ( 'NONE', #3026, #9812, #4472, .T. ) ;
#13205 = APPLICATION_PROTOCOL_DEFINITION ( 'draft international standard', 'automotive_design', 1998, #713 ) ;
#13206 = CIRCLE ( 'NONE', #13711, 1.700000000000000178 ) ;
#13207 = CARTESIAN_POINT ( 'NONE',  ( 0.000000000000000000, 6.928203230275514990, -4.000000000000003553 ) ) ;
#13208 = CARTESIAN_POINT ( 'NONE',  ( 201.2658342953964166, 49.58143373454755931, -3.806719548689701416 ) ) ;
#13209 = ORIENTED_EDGE ( 'NONE', *, *, #9420, .F. ) ;
#13210 = DIRECTION ( 'NONE',  ( 0.000000000000000000, 1.000000000000000000, 6.938893903907227145E-17 ) ) ;
#13211 = DIRECTION ( 'NONE',  ( 0.7071067811864983899, 0.000000000000000000, 0.7071067811865966446 ) ) ;
#13212 = CARTESIAN_POINT ( 'NONE',  ( -179.1973253475678121, 117.8771479419235675, 5.305259944336949474 ) ) ;
#13213 = DIRECTION ( 'NONE',  ( 0.000000000000000000, 1.734723475976806306E-15, -1.000000000000000000 ) ) ;
#13214 = ORIENTED_EDGE ( 'NONE', *, *, #4084, .F. ) ;
#13215 = CARTESIAN_POINT ( 'NONE',  ( -175.8063512637129975, 129.6626919947313468, 7.909502539118761888 ) ) ;
#13216 = CARTESIAN_POINT ( 'NONE',  ( 191.3918663844754349, 39.68659111044760124, -5.934329888686073140 ) ) ;
#13217 = ORIENTED_EDGE ( 'NONE', *, *, #12205, .F. ) ;
#13218 = ORIENTED_EDGE ( 'NONE', *, *, #6928, .T. ) ;
#13219 = LINE ( 'NONE', #9611, #4282 ) ;
#13220 = CARTESIAN_POINT ( 'NONE',  ( 177.5000000000000853, 15.53993994372673981, -17.50000000000002487 ) ) ;
#13221 = CONICAL_SURFACE ( 'NONE', #1634, 3.525000000000000355, 0.7853981633975176679 ) ;
#13222 = FACE_OUTER_BOUND ( 'NONE', #11763, .T. ) ;
#13223 = DIRECTION ( 'NONE',  ( 0.000000000000000000, 4.956352788505162775E-17, -1.000000000000000000 ) ) ;
#13224 = CARTESIAN_POINT ( 'NONE',  ( -64.00000000000002842, 14.97035339324670744, 37.58005016923963382 ) ) ;
#13225 = EDGE_CURVE ( 'NONE', #9422, #6607, #11678, .T. ) ;
#13226 = CARTESIAN_POINT ( 'NONE',  ( -220.7075610805327415, 147.6932589714580217, 9.903996657696321648 ) ) ;
#13227 = DIRECTION ( 'NONE',  ( -0.000000000000000000, 1.000000000000000000, -0.000000000000000000 ) ) ;
#13228 = CARTESIAN_POINT ( 'NONE',  ( -155.7733134923769569, 109.6950568002141324, 9.581378567423390891 ) ) ;
#13229 = CIRCLE ( 'NONE', #361, 1.000000000000000000 ) ;
#13230 = CARTESIAN_POINT ( 'NONE',  ( -214.8715905313398480, 153.8675021612092451, 2.500000000000000000 ) ) ;
#13231 = CARTESIAN_POINT ( 'NONE',  ( -35.99999999999995026, 56.53993994372675047, 16.70000000000140261 ) ) ;
#13232 = CARTESIAN_POINT ( 'NONE',  ( 163.9288925978260352, 14.41035391906035201, -6.370175303308202253 ) ) ;
#13233 = ORIENTED_EDGE ( 'NONE', *, *, #3272, .T. ) ;
#13234 = EDGE_CURVE ( 'NONE', #10742, #12734, #12427, .T. ) ;
#13235 =( LENGTH_UNIT ( ) NAMED_UNIT ( * ) SI_UNIT ( .MILLI., .METRE. ) );
#13236 = ORIENTED_EDGE ( 'NONE', *, *, #2371, .T. ) ;
#13237 = CARTESIAN_POINT ( 'NONE',  ( -76.00000000000001421, 16.03993994372673981, 24.94742576086838781 ) ) ;
#13238 = DIRECTION ( 'NONE',  ( -1.000000000000000000, -0.000000000000000000, -0.000000000000000000 ) ) ;
#13239 = FILL_AREA_STYLE ('',( #2599 ) ) ;
#13240 = LINE ( 'NONE', #7497, #1836 ) ;
#13241 = CARTESIAN_POINT ( 'NONE',  ( -172.4898389879764409, 113.0345383165057314, 2.431557144026070372 ) ) ;
#13242 = EDGE_CURVE ( 'NONE', #234, #10853, #4620, .T. ) ;
#13243 = DIRECTION ( 'NONE',  ( 0.000000000000000000, 0.000000000000000000, 1.000000000000000000 ) ) ;
#13244 = CARTESIAN_POINT ( 'NONE',  ( 120.8806775638430224, 45.00321902537314145, 7.600000000000002309 ) ) ;
#13245 = AXIS2_PLACEMENT_3D ( 'NONE', #14130, #14361, #3325 ) ;
#13246 = EDGE_LOOP ( 'NONE', ( #14010, #2841, #11056, #3809 ) ) ;
#13247 = EDGE_CURVE ( 'NONE', #1565, #6421, #5634, .T. ) ;
#13248 = ORIENTED_EDGE ( 'NONE', *, *, #13247, .F. ) ;
#13249 = LINE ( 'NONE', #2132, #7626 ) ;
#13250 = VERTEX_POINT ( 'NONE', #4401 ) ;
#13251 = CARTESIAN_POINT ( 'NONE',  ( -224.0093084580825575, 145.8913731604616828, 8.788474005012725243 ) ) ;
#13252 = ORIENTED_EDGE ( 'NONE', *, *, #9696, .T. ) ;
#13253 = ORIENTED_EDGE ( 'NONE', *, *, #6979, .T. ) ;
#13254 = DIRECTION ( 'NONE',  ( 1.000000000000000000, 0.000000000000000000, 0.000000000000000000 ) ) ;
#13255 = AXIS2_PLACEMENT_3D ( 'NONE', #7720, #6217, #2659 ) ;
#13256 = ORIENTED_EDGE ( 'NONE', *, *, #839, .F. ) ;
#13257 = DIRECTION ( 'NONE',  ( -0.000000000000000000, -0.000000000000000000, 1.000000000000000000 ) ) ;
#13258 = DIRECTION ( 'NONE',  ( 0.4873681696970831312, 0.8731965799097676229, 0.000000000000000000 ) ) ;
#13259 = DIRECTION ( 'NONE',  ( 0.000000000000000000, 0.000000000000000000, 1.000000000000000000 ) ) ;
#13260 = EDGE_CURVE ( 'NONE', #14171, #9678, #14439, .T. ) ;
#13262 = EDGE_CURVE ( 'NONE', #4290, #10772, #6714, .T. ) ;
#13261 = ADVANCED_FACE ( 'NONE', ( #14028 ), #920, .F. ) ;
#13263 = AXIS2_PLACEMENT_3D ( 'NONE', #6760, #7952, #5332 ) ;
#13264 = ORIENTED_EDGE ( 'NONE', *, *, #5883, .T. ) ;
#13265 = DIRECTION ( 'NONE',  ( 0.000000000000000000, -1.000000000000000000, -1.156482317317871478E-16 ) ) ;
#13266 = EDGE_CURVE ( 'NONE', #12618, #9525, #4370, .T. ) ;
#13267 = ORIENTED_EDGE ( 'NONE', *, *, #10376, .F. ) ;
#13268 = DIRECTION ( 'NONE',  ( -0.000000000000000000, 1.000000000000000000, -0.000000000000000000 ) ) ;
#13269 = CARTESIAN_POINT ( 'NONE',  ( 184.0000000000000568, -201.3058001507315566, -41.45141194869120227 ) ) ;
#13270 = CARTESIAN_POINT ( 'NONE',  ( -150.5371985203381087, 107.7812629986988782, -4.939346198087218198 ) ) ;
#13271 = EDGE_LOOP ( 'NONE', ( #8677, #6226, #6976, #2234 ) ) ;
#13272 = ORIENTED_EDGE ( 'NONE', *, *, #2131, .F. ) ;
#13273 = CARTESIAN_POINT ( 'NONE',  ( -207.1016862382755335, 146.9901175548950505, -2.963320117457100888 ) ) ;
#13274 = CARTESIAN_POINT ( 'NONE',  ( 190.6221111713484788, 48.05726534264031358, -4.889407597981446862 ) ) ;
#13275 = ORIENTED_EDGE ( 'NONE', *, *, #253, .T. ) ;
#13276 = FACE_BOUND ( 'NONE', #6442, .T. ) ;
#13277 = DIRECTION ( 'NONE',  ( 0.000000000000000000, -0.000000000000000000, 1.000000000000000000 ) ) ;
#13278 = CARTESIAN_POINT ( 'NONE',  ( 178.0000000000000853, 13.40307322461931072, 37.29540324609171620 ) ) ;
#13279 = ADVANCED_FACE ( 'NONE', ( #10889 ), #3612, .F. ) ;
#13280 = ORIENTED_EDGE ( 'NONE', *, *, #14143, .T. ) ;
#13281 =( LENGTH_UNIT ( ) NAMED_UNIT ( * ) SI_UNIT ( .MILLI., .METRE. ) );
#13282 = CARTESIAN_POINT ( 'NONE',  ( 207.1690005588685040, 46.08364065960329725, 0.3832845883476674320 ) ) ;
#13283 = ORIENTED_EDGE ( 'NONE', *, *, #6341, .T. ) ;
#13284 = DIRECTION ( 'NONE',  ( 1.000000000000000000, 0.000000000000000000, 0.000000000000000000 ) ) ;
#13285 = DIRECTION ( 'NONE',  ( -5.518327896226364679E-17, -0.9902680687415713612, 0.1391731009600582492 ) ) ;
#13286 = AXIS2_PLACEMENT_3D ( 'NONE', #7187, #15358, #7022 ) ;
#13287 = ADVANCED_FACE ( 'NONE', ( #14181 ), #5982, .T. ) ;
#13288 = CARTESIAN_POINT ( 'NONE',  ( -209.4369489341841586, 132.9646294043573675, 3.478895870929508582 ) ) ;
#13289 = CARTESIAN_POINT ( 'NONE',  ( 178.0000000000000853, 14.90076684276668040, -2.084916134869000182 ) ) ;
#13290 = ORIENTED_EDGE ( 'NONE', *, *, #4008, .F. ) ;
#13291 = B_SPLINE_CURVE_WITH_KNOTS ( 'NONE', 3,
 ( #11239, #3450, #8281, #11898, #8878, #8958, #4121, #5477, #3027, #12717, #11311, #10365, #6672, #4354, #13989, #4270, #9189, #5395, #9031, #1906, #7933, #13829, #15082, #6818, #7771, #5552, #471, #11394, #1752, #7858, #10215, #12644, #6744, #4044, #4192, #557, #5313, #13670, #3176, #11544, #709, #10056, #9113, #15159 ),
 .UNSPECIFIED., .F., .F.,
 ( 4, 2, 2, 2, 2, 2, 2, 2, 2, 2, 2, 2, 2, 2, 2, 2, 2, 2, 2, 2, 2, 4 ),
 ( 0.000000000000000000, 0.01154246058414762008, 0.06319472280952896648, 0.1156547325041140800, 0.1678637871092111822, 0.2189476930995808979, 0.2714221776790743945, 0.3227197530690046334, 0.3747274728241424824, 0.4267432521036158555, 0.4780248536244998681, 0.5305055628088307662, 0.5815973485975094448, 0.6337991395759137170, 0.6855599279679012170, 0.7371634071600560167, 0.7894711232639126663, 0.8405207634104210346, 0.8929453349049019106, 0.9452650328228678900, 0.9965476795071586125, 1.000000000000000000 ),
 .UNSPECIFIED. ) ;
#13292 = CARTESIAN_POINT ( 'NONE',  ( -208.4664676862339832, 144.5514869593766036, 9.578254705571838556 ) ) ;
#13293 = DIRECTION ( 'NONE',  ( -0.000000000000000000, -0.000000000000000000, 1.000000000000000000 ) ) ;
#13294 = ORIENTED_EDGE ( 'NONE', *, *, #2642, .T. ) ;
#13295 = VERTEX_POINT ( 'NONE', #5824 ) ;
#13296 = DIRECTION ( 'NONE',  ( -0.000000000000000000, -0.000000000000000000, 1.000000000000000000 ) ) ;
#13297 = CARTESIAN_POINT ( 'NONE',  ( -35.99999999999995026, 64.53993994372673626, 11.47500000000139941 ) ) ;
#13298 = ADVANCED_FACE ( 'NONE', ( #12054 ), #11942, .F. ) ;
#13299 = CONICAL_SURFACE ( 'NONE', #12793, 3.525000000000000355, 0.7853981633973787790 ) ;
#13300 = CARTESIAN_POINT ( 'NONE',  ( -63.50000000000002842, 14.90076684276667862, -2.084916134868993076 ) ) ;
#13301 = CARTESIAN_POINT ( 'NONE',  ( 200.1062858801516597, 40.86394065090267702, 16.00000000000001421 ) ) ;
#13302 = CARTESIAN_POINT ( 'NONE',  ( -223.5670544175258101, 142.1005145561789789, 1.135202858279962701 ) ) ;
#13303 = VECTOR ( 'NONE', #9624, 1000.000000000000000 ) ;
#13304 = DIRECTION ( 'NONE',  ( 1.000000000000000000, 0.000000000000000000, 0.000000000000000000 ) ) ;
#13305 = FACE_OUTER_BOUND ( 'NONE', #14527, .T. ) ;
#13306 = CARTESIAN_POINT ( 'NONE',  ( -76.50000000000001421, -181.3058001507315566, -51.45141194869120227 ) ) ;
#13307 = LINE ( 'NONE', #10966, #1456 ) ;
#13308 = DIRECTION ( 'NONE',  ( 0.000000000000000000, 0.000000000000000000, 1.000000000000000000 ) ) ;
#13309 = PRODUCT_DEFINITION_FORMATION_WITH_SPECIFIED_SOURCE ( 'ANY', '', #12937, .NOT_KNOWN. ) ;
#13310 = VERTEX_POINT ( 'NONE', #7259 ) ;
#13311 = CARTESIAN_POINT ( 'NONE',  ( 0.2456200930618607225, -3.175426480542939967, 2.004439700231694701E-16 ) ) ;
#13312 = VECTOR ( 'NONE', #13537, 1000.000000000000000 ) ;
#13313 =( LENGTH_UNIT ( ) NAMED_UNIT ( * ) SI_UNIT ( .MILLI., .METRE. ) );
#13314 = ORIENTED_EDGE ( 'NONE', *, *, #10370, .T. ) ;
#13315 = DIRECTION ( 'NONE',  ( 0.000000000000000000, -1.000000000000000000, 0.000000000000000000 ) ) ;
#13316 = CARTESIAN_POINT ( 'NONE',  ( 114.0000000000000568, 62.13993994372673768, 13.30000000000035776 ) ) ;
#13317 = DIRECTION ( 'NONE',  ( 0.000000000000000000, -1.734723475976808672E-15, -1.000000000000000000 ) ) ;
#13318 = CARTESIAN_POINT ( 'NONE',  ( 184.0000000000000568, 17.53993994372673981, -12.49999999999999467 ) ) ;
#13319 = FACE_BOUND ( 'NONE', #509, .T. ) ;
#13320 = ADVANCED_FACE ( 'NONE', ( #6070 ), #2503, .F. ) ;
#13321 = LINE ( 'NONE', #14504, #8079 ) ;
#13322 = CARTESIAN_POINT ( 'NONE',  ( -198.5677679834141713, 144.7676449960911498, 2.500000000000000000 ) ) ;
#13323 = CIRCLE ( 'NONE', #12285, 1.000000000000000888 ) ;
#13324 = ORIENTED_EDGE ( 'NONE', *, *, #8264, .T. ) ;
#13325 = AXIS2_PLACEMENT_3D ( 'NONE', #15500, #3441, #9291 ) ;
#13326 = ORIENTED_EDGE ( 'NONE', *, *, #14788, .T. ) ;
#13327 = CARTESIAN_POINT ( 'NONE',  ( 208.8071490909987347, 39.71769555335276891, -3.129532392942456553 ) ) ;
#13328 = CARTESIAN_POINT ( 'NONE',  ( 68.56535645333921991, 38.79159067395544014, 7.600000000000002309 ) ) ;
#13329 = VERTEX_POINT ( 'NONE', #4713 ) ;
#13330 = CARTESIAN_POINT ( 'NONE',  ( -222.4858765390136455, 148.6208405819451173, 7.858754932069772714 ) ) ;
#13331 = EDGE_LOOP ( 'NONE', ( #8800, #66, #11253, #6809 ) ) ;
#13332 = CARTESIAN_POINT ( 'NONE',  ( 174.2293059057019775, 61.25683321636181233, 0.000000000000000000 ) ) ;
#13333 = CARTESIAN_POINT ( 'NONE',  ( 207.3463650020273974, 50.30900816961851518, -7.069655767765518739 ) ) ;
#13334 = AXIS2_PLACEMENT_3D ( 'NONE', #10779, #14541, #5007 ) ;
#13335 = CIRCLE ( 'NONE', #6290, 1.700000000000007061 ) ;
#13336 = EDGE_CURVE ( 'NONE', #9376, #11059, #13955, .T. ) ;
#13337 = ORIENTED_EDGE ( 'NONE', *, *, #856, .F. ) ;
#13338 = CARTESIAN_POINT ( 'NONE',  ( -150.4086188282879277, 107.2728346664360259, 9.719846845941791713 ) ) ;
#13339 = DIRECTION ( 'NONE',  ( 0.000000000000000000, 0.000000000000000000, 1.000000000000000000 ) ) ;
#13340 = FACE_OUTER_BOUND ( 'NONE', #9668, .T. ) ;
#13341 = ORIENTED_EDGE ( 'NONE', *, *, #6901, .F. ) ;
#13342 = CIRCLE ( 'NONE', #13856, 5.000000000000017764 ) ;
#13343 = AXIS2_PLACEMENT_3D ( 'NONE', #1248, #12148, #1326 ) ;
#13344 = AXIS2_PLACEMENT_3D ( 'NONE', #8883, #6439, #1759 ) ;
#13345 = ORIENTED_EDGE ( 'NONE', *, *, #4302, .F. ) ;
#13346 = FACE_OUTER_BOUND ( 'NONE', #6922, .T. ) ;
#13347 = ORIENTED_EDGE ( 'NONE', *, *, #5273, .T. ) ;
#13348 = EDGE_CURVE ( 'NONE', #7455, #4643, #13449, .T. ) ;
#13349 = CARTESIAN_POINT ( 'NONE',  ( 114.0000000000000568, 59.53993994372674337, 15.00000000000035172 ) ) ;
#13350 = CARTESIAN_POINT ( 'NONE',  ( 178.0000000000000853, 16.03993994372673626, 52.49999999999997868 ) ) ;
#13351 = CIRCLE ( 'NONE', #12858, 3.499999999999996003 ) ;
#13352 = ORIENTED_EDGE ( 'NONE', *, *, #5928, .T. ) ;
#13353 = ORIENTED_EDGE ( 'NONE', *, *, #7777, .F. ) ;
#13354 = CARTESIAN_POINT ( 'NONE',  ( -179.6520503532206021, 128.8169225571170102, -4.640918829492417075 ) ) ;
#13355 = CARTESIAN_POINT ( 'NONE',  ( 0.2456200930618607225, -3.175426480542939967, 2.004439700231694701E-16 ) ) ;
#13356 = CIRCLE ( 'NONE', #12603, 4.999999999999990230 ) ;
#13357 = EDGE_CURVE ( 'NONE', #6332, #12823, #14415, .T. ) ;
#13358 = ORIENTED_EDGE ( 'NONE', *, *, #10684, .F. ) ;
#13359 = AXIS2_PLACEMENT_3D ( 'NONE', #12509, #1697, #2737 ) ;
#13360 = EDGE_CURVE ( 'NONE', #5662, #13310, #3630, .T. ) ;
#13361 = DIRECTION ( 'NONE',  ( 0.000000000000000000, 0.000000000000000000, 1.000000000000000000 ) ) ;
#13362 = CARTESIAN_POINT ( 'NONE',  ( 172.5293059057019889, 61.25683321636181233, 10.00000000000000178 ) ) ;
#13363 = EDGE_CURVE ( 'NONE', #14309, #6660, #2622, .T. ) ;
#13364 = FACE_OUTER_BOUND ( 'NONE', #13037, .T. ) ;
#13365 = ORIENTED_EDGE ( 'NONE', *, *, #3762, .T. ) ;
#13366 = VECTOR ( 'NONE', #6029, 1000.000000000000000 ) ;
#13367 = DIRECTION ( 'NONE',  ( 0.000000000000000000, -0.1391731009600592484, 0.9902680687415712502 ) ) ;
#13368 = CARTESIAN_POINT ( 'NONE',  ( 194.8975446553719451, 47.93174114899129989, -1.867390259657528251 ) ) ;
#13369 = ORIENTED_EDGE ( 'NONE', *, *, #8208, .F. ) ;
#13370 = LINE ( 'NONE', #8502, #14148 ) ;
#13371 = CARTESIAN_POINT ( 'NONE',  ( -76.50000000000004263, -179.8058001507315566, 84.88378295107887084 ) ) ;
#13372 = CARTESIAN_POINT ( 'NONE',  ( -222.0824530901772675, 149.3436370173336059, -5.265047855996057180 ) ) ;
#13373 = DIRECTION ( 'NONE',  ( -0.000000000000000000, 0.000000000000000000, 1.000000000000000000 ) ) ;
#13374 = ORIENTED_EDGE ( 'NONE', *, *, #2683, .T. ) ;
#13375 = CARTESIAN_POINT ( 'NONE',  ( -187.1267843490969369, 133.7770572797440991, 9.578254705571838556 ) ) ;
#13376 = CARTESIAN_POINT ( 'NONE',  ( 193.1007612367029367, 46.15997280778478995, -6.307360761128419036 ) ) ;
#13377 = EDGE_CURVE ( 'NONE', #8299, #5720, #13068, .T. ) ;
#13378 = EDGE_CURVE ( 'NONE', #2448, #5048, #10199, .T. ) ;
#13379 = ORIENTED_EDGE ( 'NONE', *, *, #8462, .F. ) ;
#13380 = ADVANCED_FACE ( 'NONE', ( #1081 ), #329, .T. ) ;
#13381 = VERTEX_POINT ( 'NONE', #8218 ) ;
#13382 = CARTESIAN_POINT ( 'NONE',  ( -201.1639158238212417, 128.1956685377806764, 2.431555724346862402 ) ) ;
#13383 = DIRECTION ( 'NONE',  ( -0.9741547192086867923, 0.2258817899775115157, 1.688901894271609290E-28 ) ) ;
#13384 = AXIS2_PLACEMENT_3D ( 'NONE', #10283, #4268, #12791 ) ;
#13385 = CARTESIAN_POINT ( 'NONE',  ( 0.01678220609566356131, 0.7854258609844410044, 8.000000000000008882 ) ) ;
#13386 = DIRECTION ( 'NONE',  ( 1.000000000000000000, 0.000000000000000000, 0.000000000000000000 ) ) ;
#13387 = DIRECTION ( 'NONE',  ( 1.000000000000000000, 0.000000000000000000, 0.000000000000000000 ) ) ;
#13388 = CARTESIAN_POINT ( 'NONE',  ( -63.50000000000002842, 14.90076684276667862, 37.08491613486885541 ) ) ;
#13389 = AXIS2_PLACEMENT_3D ( 'NONE', #14736, #14500, #6081 ) ;
#13390 = DIRECTION ( 'NONE',  ( -0.000000000000000000, -0.000000000000000000, 1.000000000000000000 ) ) ;
#13391 = ADVANCED_FACE ( 'NONE', ( #1312 ), #10963, .F. ) ;
#13392 = FACE_BOUND ( 'NONE', #2513, .T. ) ;
#13393 = CIRCLE ( 'NONE', #11135, 3.500000000000003109 ) ;
#13394 = CYLINDRICAL_SURFACE ( 'NONE', #10119, 1.499999999999997780 ) ;
#13395 = ORIENTED_EDGE ( 'NONE', *, *, #12820, .F. ) ;
#13396 = DIRECTION ( 'NONE',  ( -0.000000000000000000, 1.000000000000000000, -0.000000000000000000 ) ) ;
#13397 = VERTEX_POINT ( 'NONE', #3456 ) ;
#13398 = LINE ( 'NONE', #4000, #6001 ) ;
#13399 = LINE ( 'NONE', #4965, #11399 ) ;
#13400 = CARTESIAN_POINT ( 'NONE',  ( -76.00000000000004263, -178.7362136002515172, 52.68580191161573367 ) ) ;
#13401 = CARTESIAN_POINT ( 'NONE',  ( 5.196152422706635576, -9.000000000000003553, 5.000000000000000000 ) ) ;
#13402 = DIRECTION ( 'NONE',  ( -1.000000000000000000, 0.000000000000000000, 0.000000000000000000 ) ) ;
#13403 = VECTOR ( 'NONE', #1647, 1000.000000000000000 ) ;
#13404 = FACE_OUTER_BOUND ( 'NONE', #86, .T. ) ;
#13405 = CARTESIAN_POINT ( 'NONE',  ( 2.000000000000000000, 1.836970198721029688E-16, -1.499999999999999778 ) ) ;
#13406 = AXIS2_PLACEMENT_3D ( 'NONE', #4565, #8225, #2274 ) ;
#13407 = ORIENTED_EDGE ( 'NONE', *, *, #7544, .F. ) ;
#13408 = CARTESIAN_POINT ( 'NONE',  ( 177.5000000000000853, 17.53993994372674692, -17.50000000000002487 ) ) ;
#13409 = EDGE_CURVE ( 'NONE', #8234, #5311, #10186, .T. ) ;
#13410 = CARTESIAN_POINT ( 'NONE',  ( 201.8629198063431716, 32.54887535240757757, -8.146526315903498627 ) ) ;
#13411 = CARTESIAN_POINT ( 'NONE',  ( -219.8226924780726392, 153.3923528764989328, 5.388728173633870355 ) ) ;
#13412 = ORIENTED_EDGE ( 'NONE', *, *, #11734, .F. ) ;
#13413 = PRESENTATION_LAYER_ASSIGNMENT (  '', '', ( #10911 ) ) ;
#13414 = CARTESIAN_POINT ( 'NONE',  ( -222.3134187894897309, 148.9298257115060551, 9.923566759394379488 ) ) ;
#13415 = ORIENTED_EDGE ( 'NONE', *, *, #5650, .T. ) ;
#13416 = DIRECTION ( 'NONE',  ( -1.000000000000000000, 0.000000000000000000, 0.000000000000000000 ) ) ;
#13418 = PRESENTATION_LAYER_ASSIGNMENT (  '', '', ( #4599 ) ) ;
#13417 = AXIS2_PLACEMENT_3D ( 'NONE', #14292, #3487, #2305 ) ;
#13419 = ORIENTED_EDGE ( 'NONE', *, *, #13363, .T. ) ;
#13420 = DIRECTION ( 'NONE',  ( 0.000000000000000000, 4.956352788505162775E-17, -1.000000000000000000 ) ) ;
#13421 = DIRECTION ( 'NONE',  ( 0.000000000000000000, 0.000000000000000000, -1.000000000000000000 ) ) ;
#13422 = DIRECTION ( 'NONE',  ( 1.000000000000000000, 0.000000000000000000, 0.000000000000000000 ) ) ;
#13423 = EDGE_LOOP ( 'NONE', ( #13026, #4298 ) ) ;
#13424 = ADVANCED_FACE ( 'NONE', ( #14723 ), #12450, .F. ) ;
#13425 = VECTOR ( 'NONE', #2913, 1000.000000000000000 ) ;
#13426 = VERTEX_POINT ( 'NONE', #6534 ) ;
#13427 = DIRECTION ( 'NONE',  ( 0.000000000000000000, 0.000000000000000000, -1.000000000000000000 ) ) ;
#13428 = EDGE_LOOP ( 'NONE', ( #11492, #12961, #3012, #864 ) ) ;
#13429 = CIRCLE ( 'NONE', #4612, 3.525000000000000355 ) ;
#13430 = PLANE ( 'NONE',  #1655 ) ;
#13431 = CARTESIAN_POINT ( 'NONE',  ( 191.4922098844999425, 60.63967129342340456, 10.00000000000000178 ) ) ;
#13432 = CARTESIAN_POINT ( 'NONE',  ( -70.00000000000000000, 17.53993994372673981, -13.99999999999999289 ) ) ;
#13433 = ORIENTED_EDGE ( 'NONE', *, *, #10920, .F. ) ;
#13434 = VERTEX_POINT ( 'NONE', #12510 ) ;
#13435 = CARTESIAN_POINT ( 'NONE',  ( -174.7802519396333878, 131.5011100042426904, 1.515441477806783066 ) ) ;
#13436 = EDGE_CURVE ( 'NONE', #8424, #14091, #8682, .T. ) ;
#13437 = CARTESIAN_POINT ( 'NONE',  ( -63.50000000000002842, 19.53993994372674692, -17.50000000000002487 ) ) ;
#13438 = EDGE_LOOP ( 'NONE', ( #9316, #11471, #9974, #9091 ) ) ;
#13439 = AXIS2_PLACEMENT_3D ( 'NONE', #11438, #2993, #12687 ) ;
#13440 = CARTESIAN_POINT ( 'NONE',  ( -157.1441973260925238, 109.3184871819199344, -4.320071790863966754 ) ) ;
#13441 = DIRECTION ( 'NONE',  ( 0.000000000000000000, 0.1391731009600592484, 0.9902680687415712502 ) ) ;
#13442 = CARTESIAN_POINT ( 'NONE',  ( 200.1062858801516597, 40.86394065090267702, 0.000000000000000000 ) ) ;
#13443 = STYLED_ITEM ( 'NONE', ( #5996 ), #5544 ) ;
#13444 = EDGE_CURVE ( 'NONE', #13055, #1161, #6295, .T. ) ;
#13445 = CARTESIAN_POINT ( 'NONE',  ( 205.5810540386909508, 47.77928077683765906, 0.5047415929677595559 ) ) ;
#13446 = VERTEX_POINT ( 'NONE', #13388 ) ;
#13447 = CARTESIAN_POINT ( 'NONE',  ( -63.50000000000002842, 15.53993994372673626, 52.49999999999997868 ) ) ;
#13448 = CARTESIAN_POINT ( 'NONE',  ( -221.7276441040589248, 145.6842803271907201, -4.311380161871197991 ) ) ;
#13449 = CIRCLE ( 'NONE', #12692, 0.5000000000000004441 ) ;
#13450 = CARTESIAN_POINT ( 'NONE',  ( -186.4817914481332366, 122.8418524018552063, -2.964974570226826867 ) ) ;
#13451 = PLANE ( 'NONE',  #10064 ) ;
#13452 = VERTEX_POINT ( 'NONE', #2739 ) ;
#13453 = CARTESIAN_POINT ( 'NONE',  ( -191.1905365997726562, 133.0085349363843363, 10.16010209732750624 ) ) ;
#13454 = CARTESIAN_POINT ( 'NONE',  ( 203.2853005557455788, 48.75346994511389198, 0.6442813861133344089 ) ) ;
#13455 = VECTOR ( 'NONE', #5415, 1000.000000000000114 ) ;
#13456 = ORIENTED_EDGE ( 'NONE', *, *, #9209, .F. ) ;
#13457 = VERTEX_POINT ( 'NONE', #7415 ) ;
#13458 = CARTESIAN_POINT ( 'NONE',  ( 164.0000000000000568, 64.53993994372673626, 13.29999999999999538 ) ) ;
#13459 = CARTESIAN_POINT ( 'NONE',  ( 169.0293059057019889, 61.25683321636181233, 10.00000000000000178 ) ) ;
#13460 = CYLINDRICAL_SURFACE ( 'NONE', #7588, 1.500000000000001332 ) ;
#13461 = AXIS2_PLACEMENT_3D ( 'NONE', #7188, #2504, #7339 ) ;
#13462 = EDGE_CURVE ( 'NONE', #14374, #10437, #9932, .T. ) ;
#13463 = FACE_OUTER_BOUND ( 'NONE', #3017, .T. ) ;
#13465 = ADVANCED_FACE ( 'NONE', ( #1699 ), #12435, .T. ) ;
#13464 = ADVANCED_FACE ( 'NONE', ( #13463 ), #7723, .T. ) ;
#13466 = PLANE ( 'NONE',  #7706 ) ;
#13467 = CARTESIAN_POINT ( 'NONE',  ( -201.8702151432138692, 146.6006509202294410, 3.478855109513426580 ) ) ;
#13468 = LINE ( 'NONE', #2743, #7784 ) ;
#13469 = FACE_BOUND ( 'NONE', #3882, .T. ) ;
#13470 = ORIENTED_EDGE ( 'NONE', *, *, #10741, .F. ) ;
#13471 = FACE_OUTER_BOUND ( 'NONE', #1238, .T. ) ;
#13472 = CIRCLE ( 'NONE', #860, 1.700000000000007061 ) ;
#13473 = ORIENTED_EDGE ( 'NONE', *, *, #13724, .T. ) ;
#13474 = CARTESIAN_POINT ( 'NONE',  ( 194.0000000000000568, 64.53993994372673626, 20.00000000000000355 ) ) ;
#13475 = DIRECTION ( 'NONE',  ( 1.000000000000000000, 0.000000000000000000, 0.000000000000000000 ) ) ;
#13476 = LINE ( 'NONE', #12291, #13127 ) ;
#13477 = CARTESIAN_POINT ( 'NONE',  ( -35.99999999999995026, 64.53993994372673626, 15.00000000000139977 ) ) ;
#13478 = DIRECTION ( 'NONE',  ( 0.000000000000000000, 0.000000000000000000, 1.000000000000000000 ) ) ;
#13479 = CARTESIAN_POINT ( 'NONE',  ( -188.8176989649505231, 137.2180184133358694, 7.919662025281898998 ) ) ;
#13480 = EDGE_LOOP ( 'NONE', ( #4113, #4407, #10926, #19 ) ) ;
#13481 = AXIS2_PLACEMENT_3D ( 'NONE', #5093, #6207, #10067 ) ;
#13482 = CARTESIAN_POINT ( 'NONE',  ( -70.00000000000000000, 15.53993994372673981, -13.99999999999999112 ) ) ;
#13483 = DIRECTION ( 'NONE',  ( 0.000000000000000000, -6.938893903907227145E-17, 1.000000000000000000 ) ) ;
#13484 = CARTESIAN_POINT ( 'NONE',  ( -219.6568521205180957, 153.6894819096027049, 4.764702133902800618 ) ) ;
#13485 = ORIENTED_EDGE ( 'NONE', *, *, #310, .T. ) ;
#13486 = CARTESIAN_POINT ( 'NONE',  ( -217.2009144557466129, 154.0222411784483825, 6.228828271822901996 ) ) ;
#13487 = VERTEX_POINT ( 'NONE', #7482 ) ;
#13488 = FACE_OUTER_BOUND ( 'NONE', #15569, .T. ) ;
#13489 = CARTESIAN_POINT ( 'NONE',  ( 201.6633919852714030, 52.66288709485617403, -3.813211015790380909 ) ) ;
#13490 = CIRCLE ( 'NONE', #12736, 1.000000000000000888 ) ;
#13491 = ORIENTED_EDGE ( 'NONE', *, *, #7204, .T. ) ;
#13492 =( REPRESENTATION_RELATIONSHIP ('NONE','NONE', #3298, #7041 ) REPRESENTATION_RELATIONSHIP_WITH_TRANSFORMATION ( #12704 )SHAPE_REPRESENTATION_RELATIONSHIP( ) );
#13493 = LINE ( 'NONE', #14753, #4729 ) ;
#13494 = CARTESIAN_POINT ( 'NONE',  ( -76.00000000000001421, 15.53993994372673981, -17.50000000000002487 ) ) ;
#13495 = EDGE_CURVE ( 'NONE', #13816, #295, #4954, .T. ) ;
#13496 = CARTESIAN_POINT ( 'NONE',  ( 175.9483885134608272, 15.03993994372673981, -3.075184203610571654 ) ) ;
#13497 = ORIENTED_EDGE ( 'NONE', *, *, #7017, .F. ) ;
#13498 = CIRCLE ( 'NONE', #12996, 10.97218105532926558 ) ;
#13499 = ORIENTED_EDGE ( 'NONE', *, *, #2188, .T. ) ;
#13500 = DIRECTION ( 'NONE',  ( 3.965082230804130220E-16, -1.486905836551548832E-16, 1.000000000000000000 ) ) ;
#13501 = CARTESIAN_POINT ( 'NONE',  ( -156.4030783857536449, 111.1758453407123852, 9.821053999514624877 ) ) ;
#13502 = ORIENTED_EDGE ( 'NONE', *, *, #3354, .T. ) ;
#13503 = DIRECTION ( 'NONE',  ( -1.000000000000000000, -0.000000000000000000, -0.000000000000000000 ) ) ;
#13504 = CIRCLE ( 'NONE', #15268, 9.999999999999994671 ) ;
#13505 = DIRECTION ( 'NONE',  ( -0.000000000000000000, -0.000000000000000000, -1.000000000000000000 ) ) ;
#13506 = EDGE_LOOP ( 'NONE', ( #9148, #1336 ) ) ;
#13507 = VERTEX_POINT ( 'NONE', #9858 ) ;
#13508 = CARTESIAN_POINT ( 'NONE',  ( 177.5000000000000853, 15.03993994372673981, -3.075184203610571654 ) ) ;
#13509 = CARTESIAN_POINT ( 'NONE',  ( 207.1325720688761294, 35.61275714886660637, -4.804596322733623914 ) ) ;
#13510 = ORIENTED_EDGE ( 'NONE', *, *, #4068, .F. ) ;
#13511 = EDGE_CURVE ( 'NONE', #295, #14046, #3377, .T. ) ;
#13512 = DIRECTION ( 'NONE',  ( 0.000000000000000000, 0.000000000000000000, 1.000000000000000000 ) ) ;
#13513 = DIRECTION ( 'NONE',  ( 0.000000000000000000, 0.000000000000000000, 1.000000000000000000 ) ) ;
#13514 = VECTOR ( 'NONE', #13548, 1000.000000000000000 ) ;
#13515 = CARTESIAN_POINT ( 'NONE',  ( 0.000000000000000000, 0.000000000000000000, 1.499999999999999778 ) ) ;
#13516 = AXIS2_PLACEMENT_3D ( 'NONE', #4293, #1924, #733 ) ;
#13517 = EDGE_CURVE ( 'NONE', #8751, #10266, #8445, .T. ) ;
#13518 = CARTESIAN_POINT ( 'NONE',  ( -64.00000000000002842, 21.51947656765318229, 9.953386152224130257 ) ) ;
#13519 = CARTESIAN_POINT ( 'NONE',  ( 198.9622538275367845, 49.57425033952682014, -2.112703922695001513 ) ) ;
#13520 = ORIENTED_EDGE ( 'NONE', *, *, #4021, .F. ) ;
#13521 = SURFACE_SIDE_STYLE ('',( #15227 ) ) ;
#13522 = CARTESIAN_POINT ( 'NONE',  ( -217.3713917269321598, 153.7233570374494320, -1.908609582020496021 ) ) ;
#13523 = CARTESIAN_POINT ( 'NONE',  ( -171.9831566630682858, 119.3897064310878875, -4.822481523602708542 ) ) ;
#13524 = FACE_OUTER_BOUND ( 'NONE', #260, .T. ) ;
#13525 = ORIENTED_EDGE ( 'NONE', *, *, #11983, .T. ) ;
#13526 = CARTESIAN_POINT ( 'NONE',  ( -225.5658467874630446, 143.1025904080742919, 5.367833425961707761 ) ) ;
#13527 = CARTESIAN_POINT ( 'NONE',  ( 207.0703735592109069, 35.50494473061488065, -6.238171316985951620 ) ) ;
#13528 = ORIENTED_EDGE ( 'NONE', *, *, #5615, .T. ) ;
#13529 = ORIENTED_EDGE ( 'NONE', *, *, #6575, .T. ) ;
#13530 = EDGE_CURVE ( 'NONE', #3126, #13507, #1626, .T. ) ;
#13531 = DIRECTION ( 'NONE',  ( 0.000000000000000000, -1.000000000000000000, -1.156482317317871478E-16 ) ) ;
#13532 = CARTESIAN_POINT ( 'NONE',  ( 164.0000000000000568, 64.51493994372674479, 18.50000000000000711 ) ) ;
#13533 = FACE_OUTER_BOUND ( 'NONE', #2751, .T. ) ;
#13534 = DIRECTION ( 'NONE',  ( 0.000000000000000000, 0.000000000000000000, -1.000000000000000000 ) ) ;
#13535 = CARTESIAN_POINT ( 'NONE',  ( -136.9508382163321585, 108.2653706395415583, 0.000000000000000000 ) ) ;
#13536 = CARTESIAN_POINT ( 'NONE',  ( -174.7889847475609599, 131.4854638080208247, 3.478855109783925315 ) ) ;
#13537 = DIRECTION ( 'NONE',  ( 1.000000000000000000, 0.000000000000000000, 0.000000000000000000 ) ) ;
#13538 = FACE_OUTER_BOUND ( 'NONE', #12401, .T. ) ;
#13539 = ORIENTED_EDGE ( 'NONE', *, *, #9571, .T. ) ;
#13540 = ADVANCED_FACE ( 'NONE', ( #7563 ), #12362, .T. ) ;
#13541 = CARTESIAN_POINT ( 'NONE',  ( 184.0000000000000568, 15.53993994372673981, -12.49999999999999289 ) ) ;
#13542 = ORIENTED_EDGE ( 'NONE', *, *, #10269, .T. ) ;
#13543 = VERTEX_POINT ( 'NONE', #14649 ) ;
#13544 = CARTESIAN_POINT ( 'NONE',  ( -150.4086188282876719, 107.4026543836269525, 9.747367390575380597 ) ) ;
#13545 = LINE ( 'NONE', #10022, #7024 ) ;
#13546 = AXIS2_PLACEMENT_3D ( 'NONE', #14453, #5940, #3647 ) ;
#13547 = CARTESIAN_POINT ( 'NONE',  ( -63.50000000000002842, -179.8058001507315566, 64.88378295107887084 ) ) ;
#13548 = DIRECTION ( 'NONE',  ( 3.965082230804130220E-16, 1.486905836551548832E-16, -1.000000000000000000 ) ) ;
#13549 = EDGE_CURVE ( 'NONE', #7275, #4775, #12434, .T. ) ;
#13550 = EDGE_CURVE ( 'NONE', #10201, #4972, #11444, .T. ) ;
#13551 = LINE ( 'NONE', #4813, #11100 ) ;
#13552 = CARTESIAN_POINT ( 'NONE',  ( -172.5511497006709192, 129.7930440361603246, 5.430596897033706405 ) ) ;
#13553 = EDGE_CURVE ( 'NONE', #8109, #6130, #1546, .T. ) ;
#13554 = ORIENTED_EDGE ( 'NONE', *, *, #13247, .T. ) ;
#13555 = CIRCLE ( 'NONE', #12312, 8.000000000000028422 ) ;
#13556 = FACE_OUTER_BOUND ( 'NONE', #4925, .T. ) ;
#13557 = AXIS2_PLACEMENT_3D ( 'NONE', #10241, #13866, #3129 ) ;
#13558 = CARTESIAN_POINT ( 'NONE',  ( 7.572474548453445031E-16, 0.2688604483138313794, -2.750000000000000888 ) ) ;
#13559 = CARTESIAN_POINT ( 'NONE',  ( -224.1569016198369297, 145.6269368429599638, 5.559760092157292277 ) ) ;
#13560 = ORIENTED_EDGE ( 'NONE', *, *, #5843, .F. ) ;
#13561 = CARTESIAN_POINT ( 'NONE',  ( -222.1447695234329842, 149.2319873451267824, 7.942449175544537887 ) ) ;
#13562 = EDGE_LOOP ( 'NONE', ( #12860, #11040, #7367, #1162 ) ) ;
#13563 = CARTESIAN_POINT ( 'NONE',  ( -35.99999999999995026, 64.51493994372674479, 11.50000000000139622 ) ) ;
#13564 = CARTESIAN_POINT ( 'NONE',  ( 198.4664250651615021, 52.63210452169714415, -3.691074174585086798 ) ) ;
#13565 = EDGE_CURVE ( 'NONE', #5473, #5101, #8819, .T. ) ;
#13566 = EDGE_LOOP ( 'NONE', ( #15532, #11321, #3312, #8008, #6302, #11771 ) ) ;
#13567 = CIRCLE ( 'NONE', #8043, 1.000000000000000888 ) ;
#13568 = EDGE_CURVE ( 'NONE', #8250, #10019, #9681, .T. ) ;
#13569 = CARTESIAN_POINT ( 'NONE',  ( 0.7145311798161593231, -4.618802153517259867, -7.999999999999979572 ) ) ;
#13570 = CARTESIAN_POINT ( 'NONE',  ( 64.00000000000005684, 64.53993994372673626, 15.00000000000070166 ) ) ;
#13571 = VECTOR ( 'NONE', #5350, 1000.000000000000227 ) ;
#13572 =( NAMED_UNIT ( * ) PLANE_ANGLE_UNIT ( ) SI_UNIT ( $, .RADIAN. ) );
#13573 = AXIS2_PLACEMENT_3D ( 'NONE', #3517, #2099, #5968 ) ;
#13574 = FACE_OUTER_BOUND ( 'NONE', #15090, .T. ) ;
#13575 = VERTEX_POINT ( 'NONE', #12764 ) ;
#13576 = DIRECTION ( 'NONE',  ( 1.000000000000000000, 0.000000000000000000, 0.000000000000000000 ) ) ;
#13577 = ORIENTED_EDGE ( 'NONE', *, *, #8331, .F. ) ;
#13578 = CONICAL_SURFACE ( 'NONE', #14584, 2.749999999999999112, 1.047197551196600296 ) ;
#13579 = CARTESIAN_POINT ( 'NONE',  ( -76.00000000000001421, 15.03993994372673981, -2.075184203610571210 ) ) ;
#13580 = ORIENTED_EDGE ( 'NONE', *, *, #5650, .F. ) ;
#13582 = AXIS2_PLACEMENT_3D ( 'NONE', #2478, #12033, #4931 ) ;
#13581 = LINE ( 'NONE', #1351, #12988 ) ;
#13583 = ADVANCED_FACE ( 'NONE', ( #1946 ), #4162, .F. ) ;
#13584 = DIRECTION ( 'NONE',  ( 0.4873681696970816324, 0.8731965799097685110, -0.000000000000000000 ) ) ;
#13585 = ORIENTED_EDGE ( 'NONE', *, *, #4797, .T. ) ;
#13586 = ORIENTED_EDGE ( 'NONE', *, *, #9015, .T. ) ;
#13587 = DIRECTION ( 'NONE',  ( 1.000000000000000000, -0.000000000000000000, -0.000000000000000000 ) ) ;
#13588 = CARTESIAN_POINT ( 'NONE',  ( 208.8002188652075972, 39.64064887424692785, -1.560527519332197022 ) ) ;
#13589 = EDGE_LOOP ( 'NONE', ( #2795, #3461, #5462, #14480 ) ) ;
#13590 = MECHANICAL_DESIGN_GEOMETRIC_PRESENTATION_REPRESENTATION (  '', ( #3030 ), #222 ) ;
#13591 = CARTESIAN_POINT ( 'NONE',  ( -61.94838851346079167, -178.8058001507315566, -17.19066787724516843 ) ) ;
#13592 = CARTESIAN_POINT ( 'NONE',  ( 190.5000000000000568, 17.53993994372674692, -17.50000000000002487 ) ) ;
#13593 = AXIS2_PLACEMENT_3D ( 'NONE', #2638, #2714, #13512 ) ;
#13594 = CARTESIAN_POINT ( 'NONE',  ( 0.000000000000000000, 2.381569860407203532, -1.375000000000002665 ) ) ;
#13595 = DIRECTION ( 'NONE',  ( 1.000000000000000000, 0.000000000000000000, 0.000000000000000000 ) ) ;
#13596 = ADVANCED_FACE ( 'NONE', ( #6642 ), #10180, .F. ) ;
#13597 = CIRCLE ( 'NONE', #6820, 1.699999999999994849 ) ;
#13598 = ORIENTED_EDGE ( 'NONE', *, *, #229, .T. ) ;
#13599 = CARTESIAN_POINT ( 'NONE',  ( -222.6001360064667267, 143.9905737129706438, -2.961424432328688461 ) ) ;
#13600 = CONICAL_SURFACE ( 'NONE', #11865, 3.525000000000002132, 0.7853981633974482790 ) ;
#13601 = CARTESIAN_POINT ( 'NONE',  ( -173.0624365063895311, 117.4516868700737433, -3.188270265946634208 ) ) ;
#13602 = AXIS2_PLACEMENT_3D ( 'NONE', #5479, #639, #13831 ) ;
#13603 = ADVANCED_FACE ( 'NONE', ( #1802 ), #11364, .F. ) ;
#13604 = CARTESIAN_POINT ( 'NONE',  ( 20.93529453487719039, 40.04259805664093363, 10.00000000000000178 ) ) ;
#13605 = VERTEX_POINT ( 'NONE', #11281 ) ;
#13606 = CARTESIAN_POINT ( 'NONE',  ( -184.7761983179757976, 119.6423109536379883, 5.434137442415926778 ) ) ;
#13607 = VECTOR ( 'NONE', #15086, 1000.000000000000000 ) ;
#13608 = CARTESIAN_POINT ( 'NONE',  ( 208.8162124854775357, 42.04914431719598156, -1.433821094984975009 ) ) ;
#13609 = ORIENTED_EDGE ( 'NONE', *, *, #2366, .T. ) ;
#13610 = CARTESIAN_POINT ( 'NONE',  ( 122.5806775638430253, 45.00321902537314145, 9.975000000000001421 ) ) ;
#13611 = FACE_OUTER_BOUND ( 'NONE', #2713, .T. ) ;
#13612 = AXIS2_PLACEMENT_3D ( 'NONE', #9653, #2619, #14447 ) ;
#13613 = CARTESIAN_POINT ( 'NONE',  ( 178.0000000000000853, -178.8753867012115961, 64.82329228561619061 ) ) ;
#13614 = DIRECTION ( 'NONE',  ( -0.4873681696970831312, -0.8731965799097676229, 0.000000000000000000 ) ) ;
#13615 = DIRECTION ( 'NONE',  ( -0.000000000000000000, -0.000000000000000000, 1.000000000000000000 ) ) ;
#13616 = ORIENTED_EDGE ( 'NONE', *, *, #15050, .F. ) ;
#13617 = CARTESIAN_POINT ( 'NONE',  ( -35.99999999999995026, 64.53993994372673626, 16.70000000000140261 ) ) ;
#13618 = CARTESIAN_POINT ( 'NONE',  ( -193.9262940755599232, 141.6759404601118320, 5.434754235172606585 ) ) ;
#13619 = CARTESIAN_POINT ( 'NONE',  ( 215.1062858801516882, 25.86394065090268057, 18.00000000000000355 ) ) ;
#13620 = CIRCLE ( 'NONE', #11363, 1.700000000000007061 ) ;
#13621 = CARTESIAN_POINT ( 'NONE',  ( 177.5000000000000853, 17.53993994372673271, 52.49999999999997868 ) ) ;
#13622 = VERTEX_POINT ( 'NONE', #11597 ) ;
#13623 = ADVANCED_FACE ( 'NONE', ( #12458 ), #4239, .T. ) ;
#13625 = LINE ( 'NONE', #1708, #7095 ) ;
#13624 = AXIS2_PLACEMENT_3D ( 'NONE', #9295, #7006, #12752 ) ;
#13626 = ORIENTED_EDGE ( 'NONE', *, *, #6019, .T. ) ;
#13627 = ORIENTED_EDGE ( 'NONE', *, *, #8664, .T. ) ;
#13628 = CARTESIAN_POINT ( 'NONE',  ( -76.00000000000004263, -179.3058001507315566, 52.19066787724494816 ) ) ;
#13629 = DIRECTION ( 'NONE',  ( 1.000000000000000000, 0.000000000000000000, 0.000000000000000000 ) ) ;
#13630 = DIRECTION ( 'NONE',  ( 0.000000000000000000, 0.000000000000000000, -1.000000000000000000 ) ) ;
#13631 = CARTESIAN_POINT ( 'NONE',  ( 14.00000000000004086, 64.53993994372673626, 11.47500000000104947 ) ) ;
#13632 = DIRECTION ( 'NONE',  ( 0.000000000000000000, -1.000000000000000000, 0.000000000000000000 ) ) ;
#13633 = CARTESIAN_POINT ( 'NONE',  ( -218.6367072074390592, 155.5172316571506599, -0.02616420791762594927 ) ) ;
#13634 = CARTESIAN_POINT ( 'NONE',  ( -193.9262940755599232, 141.6759404601118320, 5.434754235172606585 ) ) ;
#13635 = EDGE_LOOP ( 'NONE', ( #12064, #10226, #13984, #8159, #2829, #10876 ) ) ;
#13636 = AXIS2_PLACEMENT_3D ( 'NONE', #14210, #2140, #5704 ) ;
#13637 = ADVANCED_FACE ( 'NONE', ( #605 ), #4403, .F. ) ;
#13638 = DIRECTION ( 'NONE',  ( 0.000000000000000000, 0.000000000000000000, 1.000000000000000000 ) ) ;
#13639 = CARTESIAN_POINT ( 'NONE',  ( -222.9820152130263295, 147.7319302668168177, 7.565779686223725875 ) ) ;
#13640 = ORIENTED_EDGE ( 'NONE', *, *, #1445, .T. ) ;
#13641 = CARTESIAN_POINT ( 'NONE',  ( -219.1834294040782538, 150.5104683866151731, 9.570045470580922142 ) ) ;
#13642 = ORIENTED_EDGE ( 'NONE', *, *, #11293, .T. ) ;
#13643 = CARTESIAN_POINT ( 'NONE',  ( -168.5715549668454685, 126.2102699412402700, -2.485716223453637852 ) ) ;
#13644 = DIRECTION ( 'NONE',  ( -1.000000000000000000, -2.751328491981765035E-32, 3.965082230804130220E-16 ) ) ;
#13645 = CIRCLE ( 'NONE', #1799, 1.700000000000007061 ) ;
#13646 = EDGE_LOOP ( 'NONE', ( #11458, #7853, #1494, #13948 ) ) ;
#13647 = DIRECTION ( 'NONE',  ( 0.000000000000000000, 0.000000000000000000, -1.000000000000000000 ) ) ;
#13648 = DIRECTION ( 'NONE',  ( 1.000000000000000000, 2.751328491981765035E-32, -3.965082230804130220E-16 ) ) ;
#13649 = AXIS2_PLACEMENT_3D ( 'NONE', #4904, #5131, #1569 ) ;
#13650 = PLANE ( 'NONE',  #14932 ) ;
#13651 = VERTEX_POINT ( 'NONE', #13794 ) ;
#13652 = SHAPE_REPRESENTATION ( 'Handle Grip', ( #12337 ), #4745 ) ;
#13653 =( LENGTH_UNIT ( ) NAMED_UNIT ( * ) SI_UNIT ( .MILLI., .METRE. ) );
#13654 = AXIS2_PLACEMENT_3D ( 'NONE', #582, #9212, #15029 ) ;
#13655 = ORIENTED_EDGE ( 'NONE', *, *, #12744, .F. ) ;
#13656 = EDGE_CURVE ( 'NONE', #7373, #3731, #13966, .T. ) ;
#13657 = EDGE_CURVE ( 'NONE', #13622, #9401, #15209, .T. ) ;
#13658 = DIRECTION ( 'NONE',  ( -0.000000000000000000, 1.000000000000000000, -0.000000000000000000 ) ) ;
#13659 = EDGE_CURVE ( 'NONE', #13457, #11511, #15047, .T. ) ;
#13660 = CARTESIAN_POINT ( 'NONE',  ( -157.6477983077465694, 110.1970436846184924, 9.411501811869198875 ) ) ;
#13661 = ORIENTED_EDGE ( 'NONE', *, *, #8534, .T. ) ;
#13662 = CLOSED_SHELL ( 'NONE', ( #7038, #13380, #13757, #12418, #10487, #15146, #8191, #15318, #13936, #3054, #9618, #5162, #10174, #10411, #491, #15453 ) ) ;
#13663 = CARTESIAN_POINT ( 'NONE',  ( 6.800000000000000711, 0.000000000000000000, 0.000000000000000000 ) ) ;
#13664 = DIRECTION ( 'NONE',  ( 0.000000000000000000, 4.956352788505162775E-17, -1.000000000000000000 ) ) ;
#13665 = ORIENTED_EDGE ( 'NONE', *, *, #9119, .T. ) ;
#13666 = ORIENTED_EDGE ( 'NONE', *, *, #5758, .T. ) ;
#13667 = LINE ( 'NONE', #14926, #11303 ) ;
#13668 = CARTESIAN_POINT ( 'NONE',  ( 202.8426534586648700, 48.90729187601812811, -2.475854291071949209 ) ) ;
#13669 = ORIENTED_EDGE ( 'NONE', *, *, #6930, .T. ) ;
#13670 = CARTESIAN_POINT ( 'NONE',  ( 208.8002188652075972, 39.64064887424692785, -1.560527519332197022 ) ) ;
#13671 = CARTESIAN_POINT ( 'NONE',  ( -34.79899788034579444, 48.72489408690345414, 10.00000000000000178 ) ) ;
#13672 = CARTESIAN_POINT ( 'NONE',  ( -157.6477983077465694, 110.1970436846185208, -4.548387523817069678 ) ) ;
#13673 = LINE ( 'NONE', #2878, #9477 ) ;
#13674 = AXIS2_PLACEMENT_3D ( 'NONE', #9572, #14373, #3570 ) ;
#13675 = DIRECTION ( 'NONE',  ( -0.3662838836490099337, 0.9305003370641709015, 0.002288952263120960697 ) ) ;
#13676 = EDGE_CURVE ( 'NONE', #14204, #12934, #4092, .T. ) ;
#13677 = CIRCLE ( 'NONE', #1359, 3.499999999999999556 ) ;
#13678 = DIRECTION ( 'NONE',  ( -3.965082230804130220E-16, 1.090924371466202084E-47, 1.000000000000000000 ) ) ;
#13679 = EDGE_LOOP ( 'NONE', ( #4742, #10031, #5930, #3468 ) ) ;
#13680 = CARTESIAN_POINT ( 'NONE',  ( -139.1458939983161827, 103.0129948961282054, 2.431557144026069928 ) ) ;
#13681 = CARTESIAN_POINT ( 'NONE',  ( -220.4755021374134287, 148.0753638217371702, -5.053461931965367526 ) ) ;
#13682 = CARTESIAN_POINT ( 'NONE',  ( -187.3343951027933656, 121.3449523462597313, -0.4555467707853332882 ) ) ;
#13683 = CARTESIAN_POINT ( 'NONE',  ( -35.99999999999995026, 64.53993994372673626, 13.30000000000139870 ) ) ;
#13684 = ORIENTED_EDGE ( 'NONE', *, *, #9274, .T. ) ;
#13685 = CARTESIAN_POINT ( 'NONE',  ( -213.9961813491638623, 134.6717504882919911, 3.478895870929492595 ) ) ;
#13686 = CARTESIAN_POINT ( 'NONE',  ( 208.7983505906672121, 39.57879239708907448, -2.990627279509298742 ) ) ;
#13687 = VECTOR ( 'NONE', #10333, 1000.000000000000000 ) ;
#13688 = ORIENTED_EDGE ( 'NONE', *, *, #6336, .T. ) ;
#13689 = VECTOR ( 'NONE', #5669, 1000.000000000000114 ) ;
#13690 = CYLINDRICAL_SURFACE ( 'NONE', #5903, 5.000000000000000000 ) ;
#13691 = DIRECTION ( 'NONE',  ( 0.000000000000000000, 0.8660254037844375974, -0.5000000000000018874 ) ) ;
#13692 = ADVANCED_FACE ( 'NONE', ( #7746 ), #2369, .T. ) ;
#13693 = DIRECTION ( 'NONE',  ( 0.000000000000000000, 0.000000000000000000, -1.000000000000000000 ) ) ;
#13694 = EDGE_CURVE ( 'NONE', #7467, #4995, #3077, .T. ) ;
#13695 = VECTOR ( 'NONE', #10256, 1000.000000000000000 ) ;
#13696 = DIRECTION ( 'NONE',  ( 0.000000000000000000, -1.000000000000000000, -1.156482317317871478E-16 ) ) ;
#13697 = VERTEX_POINT ( 'NONE', #6483 ) ;
#13698 = CARTESIAN_POINT ( 'NONE',  ( 194.0000000000000568, 59.53993994372674337, 10.00000000000000178 ) ) ;
#13699 = AXIS2_PLACEMENT_3D ( 'NONE', #263, #340, #11187 ) ;
#13700 =( REPRESENTATION_RELATIONSHIP ('NONE','NONE', #3298, #11876 ) REPRESENTATION_RELATIONSHIP_WITH_TRANSFORMATION ( #13977 )SHAPE_REPRESENTATION_RELATIONSHIP( ) );
#13701 = CARTESIAN_POINT ( 'NONE',  ( -207.0940556909077657, 149.0079180481279479, 5.434754235172608361 ) ) ;
#13702 = DIRECTION ( 'NONE',  ( -0.000000000000000000, 1.000000000000000000, -0.000000000000000000 ) ) ;
#13703 = CARTESIAN_POINT ( 'NONE',  ( -157.6240445055952648, 110.4483201618638191, -4.636096941365077662 ) ) ;
#13704 = VERTEX_POINT ( 'NONE', #1873 ) ;
#13706 = VECTOR ( 'NONE', #10482, 1000.000000000000000 ) ;
#13705 = CARTESIAN_POINT ( 'NONE',  ( -64.00000000000002842, 16.03993994372673981, 10.05257423913146475 ) ) ;
#13707 = ORIENTED_EDGE ( 'NONE', *, *, #855, .T. ) ;
#13708 = ORIENTED_EDGE ( 'NONE', *, *, #11049, .T. ) ;
#13709 = DIRECTION ( 'NONE',  ( 0.000000000000000000, -1.000000000000000000, 0.000000000000000000 ) ) ;
#13710 = CARTESIAN_POINT ( 'NONE',  ( -61.94838851346079167, 15.03993994372673981, -3.075184203610571654 ) ) ;
#13711 = AXIS2_PLACEMENT_3D ( 'NONE', #12402, #8708, #1586 ) ;
#13712 =( NAMED_UNIT ( * ) SI_UNIT ( $, .STERADIAN. ) SOLID_ANGLE_UNIT ( ) );
#13713 =( NAMED_UNIT ( * ) PLANE_ANGLE_UNIT ( ) SI_UNIT ( $, .RADIAN. ) );
#13714 = CARTESIAN_POINT ( 'NONE',  ( -76.00000000000004263, 15.53993994372673804, 52.49999999999997868 ) ) ;
#13715 = B_SPLINE_CURVE_WITH_KNOTS ( 'NONE', 3,
 ( #5746, #12923, #10560, #14488, #8217, #11986, #14414, #7258, #4878, #14331, #3534, #15513, #2112, #13067, #7099, #1155, #5981, #3455, #2349, #5823, #8367, #13226, #15590, #9619, #4558, #10643, #8446, #7184, #15435, #10885, #2426, #8287, #2268, #9384, #12053, #12995, #6069, #11904, #1079, #2187, #9699, #10720, #6944, #11751 ),
 .UNSPECIFIED., .F., .F.,
 ( 4, 2, 2, 2, 2, 2, 2, 2, 2, 2, 2, 2, 2, 2, 2, 2, 2, 2, 2, 2, 2, 4 ),
 ( 0.02425151066300419017, 0.02566658695633274381, 0.02708166324966130092, 0.02778920139632557254, 0.02849673954298984069, 0.02991181583631835617, 0.03132689212964687164, 0.03203443027631112938, 0.03274196842297538712, 0.03415704471630390260, 0.03557212100963242501, 0.03698719730296094743, 0.03769473544962523986, 0.03840227359628953230, 0.03981734988961815880, 0.04123242618294678530, 0.04193996432961112630, 0.04264750247627546037, 0.04406257876960419095, 0.04477011691626857359, 0.04547765506293295623, 0.04689273135626172151 ),
 .UNSPECIFIED. ) ;
#13716 = AXIS2_PLACEMENT_3D ( 'NONE', #11764, #3315, #11689 ) ;
#13717 = ORIENTED_EDGE ( 'NONE', *, *, #5674, .F. ) ;
#13718 = DIRECTION ( 'NONE',  ( 0.000000000000000000, 0.000000000000000000, 1.000000000000000000 ) ) ;
#13719 = EDGE_CURVE ( 'NONE', #13704, #14207, #4379, .T. ) ;
#13720 = AXIS2_PLACEMENT_3D ( 'NONE', #9602, #7166, #1211 ) ;
#13721 = CARTESIAN_POINT ( 'NONE',  ( 190.5000000000000568, -178.8058001507315566, -30.31842631998718574 ) ) ;
#13722 = CARTESIAN_POINT ( 'NONE',  ( -223.8893703921771419, 146.1062610326309823, -1.348932811884229421 ) ) ;
#13723 = ORIENTED_EDGE ( 'NONE', *, *, #14218, .T. ) ;
#13724 = EDGE_CURVE ( 'NONE', #9501, #14894, #10447, .T. ) ;
#13725 = CARTESIAN_POINT ( 'NONE',  ( -217.2630589882568870, 153.9147002545655027, 6.438236223713596829 ) ) ;
#13726 = ORIENTED_EDGE ( 'NONE', *, *, #6558, .F. ) ;
#13727 = CARTESIAN_POINT ( 'NONE',  ( -170.7457446375415770, 122.3148678559813476, -5.128095649471044126 ) ) ;
#13728 = LINE ( 'NONE', #14039, #1040 ) ;
#13729 = ORIENTED_EDGE ( 'NONE', *, *, #11900, .F. ) ;
#13730 = CARTESIAN_POINT ( 'NONE',  ( 2.000000000000000000, -1.587713240271461546, 2.750000000000000000 ) ) ;
#13731 = LINE ( 'NONE', #5141, #12871 ) ;
#13732 = VECTOR ( 'NONE', #8255, 1000.000000000000000 ) ;
#13733 = ADVANCED_FACE ( 'NONE', ( #11519 ), #6715, .F. ) ;
#13734 = PLANE ( 'NONE',  #13931 ) ;
#13735 = ORIENTED_EDGE ( 'NONE', *, *, #2433, .T. ) ;
#13736 = ITEM_DEFINED_TRANSFORMATION ( 'NONE', 'NONE', #14068,  #12337 ) ;
#13737 = ORIENTED_EDGE ( 'NONE', *, *, #318, .F. ) ;
#13738 = CARTESIAN_POINT ( 'NONE',  ( -156.8030008057995985, 111.1938936318135376, 9.788006227097792333 ) ) ;
#13739 = ORIENTED_EDGE ( 'NONE', *, *, #7587, .F. ) ;
#13740 = DIRECTION ( 'NONE',  ( -1.000000000000000000, -0.000000000000000000, -0.000000000000000000 ) ) ;
#13741 = DIRECTION ( 'NONE',  ( 1.000000000000000000, 0.000000000000000000, 0.000000000000000000 ) ) ;
#13742 = ORIENTED_EDGE ( 'NONE', *, *, #10888, .T. ) ;
#13743 = ORIENTED_EDGE ( 'NONE', *, *, #9302, .F. ) ;
#13744 = CARTESIAN_POINT ( 'NONE',  ( -185.2055264765504887, 137.3096093875189467, 2.500000000000000000 ) ) ;
#13745 = ADVANCED_FACE ( 'NONE', ( #7976 ), #6915, .T. ) ;
#13746 = DIRECTION ( 'NONE',  ( 0.000000000000000000, 0.000000000000000000, 1.000000000000000000 ) ) ;
#13747 = EDGE_LOOP ( 'NONE', ( #9895, #4784, #5509, #1408, #13407, #5306 ) ) ;
#13748 = CARTESIAN_POINT ( 'NONE',  ( 0.4969600502617546600, -4.995646404165271726, 7.347286611336989459 ) ) ;
#13749 = FACE_OUTER_BOUND ( 'NONE', #7135, .T. ) ;
#13750 = CARTESIAN_POINT ( 'NONE',  ( -70.00000000000000000, -179.3058001507315566, -41.45141194869120227 ) ) ;
#13751 = LINE ( 'NONE', #797, #12751 ) ;
#13753 = EDGE_CURVE ( 'NONE', #3709, #11977, #12796, .T. ) ;
#13752 = ADVANCED_FACE ( 'NONE', ( #10413 ), #12925, .F. ) ;
#13754 = EDGE_CURVE ( 'NONE', #12671, #11360, #4989, .T. ) ;
#13755 = CARTESIAN_POINT ( 'NONE',  ( -5.196152422706630247, -9.000000000000005329, 0.000000000000000000 ) ) ;
#13756 = CIRCLE ( 'NONE', #14261, 1.000000000000000888 ) ;
#13757 = ADVANCED_FACE ( 'NONE', ( #14104 ), #9286, .T. ) ;
#13758 = CIRCLE ( 'NONE', #1389, 3.500000000000003109 ) ;
#13759 = FACE_OUTER_BOUND ( 'NONE', #13810, .T. ) ;
#13760 = ORIENTED_EDGE ( 'NONE', *, *, #14370, .T. ) ;
#13761 = CARTESIAN_POINT ( 'NONE',  ( 175.9483885134608272, -179.3058001507315566, -51.45141194869120227 ) ) ;
#13762 = LINE ( 'NONE', #12569, #4923 ) ;
#13763 = CARTESIAN_POINT ( 'NONE',  ( -167.6561596704311512, 127.1594819807359329, -0.4629209656553701646 ) ) ;
#13764 = DIRECTION ( 'NONE',  ( -0.000000000000000000, -0.000000000000000000, 1.000000000000000000 ) ) ;
#13765 = ORIENTED_EDGE ( 'NONE', *, *, #8253, .F. ) ;
#13766 = CARTESIAN_POINT ( 'NONE',  ( -176.6594047394515314, 116.7136007993067324, 1.317773660835219740 ) ) ;
#13767 = CARTESIAN_POINT ( 'NONE',  ( 205.3727474927790411, 33.82195144205066839, -0.3638485434072702973 ) ) ;
#13768 = ORIENTED_EDGE ( 'NONE', *, *, #2167, .T. ) ;
#13769 = AXIS2_PLACEMENT_3D ( 'NONE', #5480, #15240, #15085 ) ;
#13770 = AXIS2_PLACEMENT_3D ( 'NONE', #7480, #1380, #14559 ) ;
#13771 = EDGE_CURVE ( 'NONE', #6271, #6990, #9536, .T. ) ;
#13772 = DIRECTION ( 'NONE',  ( -0.000000000000000000, -0.000000000000000000, 1.000000000000000000 ) ) ;
#13773 = CARTESIAN_POINT ( 'NONE',  ( 0.1085346982764772705, -1.064859738961390079, 2.750000000000000444 ) ) ;
#13774 = DIRECTION ( 'NONE',  ( 0.000000000000000000, 8.673617379884035472E-17, -1.000000000000000000 ) ) ;
#13775 = DIRECTION ( 'NONE',  ( 0.000000000000000000, 0.000000000000000000, 1.000000000000000000 ) ) ;
#13776 = VECTOR ( 'NONE', #2440, 1000.000000000000114 ) ;
#13777 = EDGE_LOOP ( 'NONE', ( #15334, #5394, #6681, #14015 ) ) ;
#13778 = FACE_OUTER_BOUND ( 'NONE', #2328, .T. ) ;
#13779 = CARTESIAN_POINT ( 'NONE',  ( -219.6650276661029011, 145.2909210783078890, 9.577123744044234499 ) ) ;
#13780 = DIRECTION ( 'NONE',  ( 0.000000000000000000, 0.000000000000000000, 1.000000000000000000 ) ) ;
#13781 = CARTESIAN_POINT ( 'NONE',  ( -156.6477983077465410, 110.1970436846185066, -5.000000000000000000 ) ) ;
#13782 = ORIENTED_EDGE ( 'NONE', *, *, #8481, .T. ) ;
#13783 = CARTESIAN_POINT ( 'NONE',  ( 0.2456200930618618050, 1.587713240271470427, 2.750000000000000888 ) ) ;
#13784 = ADVANCED_FACE ( 'NONE', ( #2192 ), #4637, .F. ) ;
#13785 = EDGE_LOOP ( 'NONE', ( #7143, #2468 ) ) ;
#13786 = VERTEX_POINT ( 'NONE', #997 ) ;
#13787 = CARTESIAN_POINT ( 'NONE',  ( -63.50000000000002842, 17.53993994372674692, -17.50000000000002487 ) ) ;
#13788 = DIRECTION ( 'NONE',  ( -0.000000000000000000, 6.938893903907227145E-17, -1.000000000000000000 ) ) ;
#13789 = DIRECTION ( 'NONE',  ( 0.4873681696970831312, 0.8731965799097676229, 0.000000000000000000 ) ) ;
#13790 = AXIS2_PLACEMENT_3D ( 'NONE', #8756, #1641, #14663 ) ;
#13791 = CARTESIAN_POINT ( 'NONE',  ( -218.7216426999998191, 155.3650563895502046, -0.4850387387758420266 ) ) ;
#13792 = FACE_OUTER_BOUND ( 'NONE', #14460, .T. ) ;
#13793 = FACE_BOUND ( 'NONE', #69, .T. ) ;
#13794 = CARTESIAN_POINT ( 'NONE',  ( 15.71029453487719074, 40.04259805664093363, 5.000000000000000000 ) ) ;
#13795 = CARTESIAN_POINT ( 'NONE',  ( 198.8863654052626657, 49.55881746625484396, -3.681704842056328086 ) ) ;
#13796 = DIRECTION ( 'NONE',  ( 0.000000000000000000, -1.000000000000000000, 0.000000000000000000 ) ) ;
#13797 = VERTEX_POINT ( 'NONE', #5983 ) ;
#13798 = VECTOR ( 'NONE', #14611, 1000.000000000000227 ) ;
#13799 = EDGE_CURVE ( 'NONE', #1426, #6169, #2972, .T. ) ;
#13800 = CARTESIAN_POINT ( 'NONE',  ( -220.5194744645034746, 152.1439585714864791, 6.950724492665587562 ) ) ;
#13801 = ORIENTED_EDGE ( 'NONE', *, *, #12594, .T. ) ;
#13802 = CARTESIAN_POINT ( 'NONE',  ( -136.9508382163321585, 108.2653706395415441, 1.734723475976807094E-15 ) ) ;
#13803 = CARTESIAN_POINT ( 'NONE',  ( 184.0000000000000568, -201.3058001507315566, -39.95141194869120937 ) ) ;
#13804 = ORIENTED_EDGE ( 'NONE', *, *, #8221, .T. ) ;
#13805 = CARTESIAN_POINT ( 'NONE',  ( -139.1458939983161827, 103.0129948961282054, 5.000000000000000000 ) ) ;
#13806 = DIRECTION ( 'NONE',  ( -0.000000000000000000, 1.000000000000000000, 1.156482317317871725E-16 ) ) ;
#13807 = PRODUCT_DEFINITION_SHAPE ( 'NONE', 'NONE',  #15629 ) ;
#13808 = AXIS2_PLACEMENT_3D ( 'NONE', #2106, #11349, #4231 ) ;
#13809 = AXIS2_PLACEMENT_3D ( 'NONE', #9260, #12948, #14284 ) ;
#13810 = EDGE_LOOP ( 'NONE', ( #3396, #13283, #9920, #1430, #13415, #3811, #14761, #14764 ) ) ;
#13811 = VECTOR ( 'NONE', #14318, 1000.000000000000000 ) ;
#13812 = CONTEXT_DEPENDENT_SHAPE_REPRESENTATION ( #4023, #4360 ) ;
#13813 = ORIENTED_EDGE ( 'NONE', *, *, #14030, .T. ) ;
#13814 = CARTESIAN_POINT ( 'NONE',  ( 207.4107378919655673, 50.26574450011962369, -5.500654858001599479 ) ) ;
#13815 = DIRECTION ( 'NONE',  ( 0.9296197478520974444, 0.3660421972118351741, -0.04266420354037655377 ) ) ;
#13816 = VERTEX_POINT ( 'NONE', #4799 ) ;
#13817 = CARTESIAN_POINT ( 'NONE',  ( 64.00000000000005684, 64.53993994372673626, 18.52500000000070202 ) ) ;
#13818 = EDGE_CURVE ( 'NONE', #4926, #828, #1196, .T. ) ;
#13819 = VECTOR ( 'NONE', #5626, 1000.000000000000000 ) ;
#13820 = DIRECTION ( 'NONE',  ( 0.000000000000000000, -1.000000000000000000, 0.000000000000000000 ) ) ;
#13821 = ORIENTED_EDGE ( 'NONE', *, *, #6433, .T. ) ;
#13822 = ORIENTED_EDGE ( 'NONE', *, *, #3089, .F. ) ;
#13823 = CARTESIAN_POINT ( 'NONE',  ( -218.4444600228138711, 155.8616726660956715, 2.500000000270498735 ) ) ;
#13824 = AXIS2_PLACEMENT_3D ( 'NONE', #2092, #4539, #4615 ) ;
#13825 = EDGE_CURVE ( 'NONE', #14046, #295, #11798, .T. ) ;
#13826 = DIRECTION ( 'NONE',  ( 0.000000000000000000, -0.9953154669545954958, -0.09668051117446378739 ) ) ;
#13827 = AXIS2_PLACEMENT_3D ( 'NONE', #13289, #11179, #331 ) ;
#13828 = VERTEX_POINT ( 'NONE', #10563 ) ;
#13829 = CARTESIAN_POINT ( 'NONE',  ( 208.8051451104704768, 39.65587490144260840, -4.559632177755815086 ) ) ;
#13830 = DIRECTION ( 'NONE',  ( -0.000000000000000000, -0.000000000000000000, 1.000000000000000000 ) ) ;
#13831 = DIRECTION ( 'NONE',  ( 0.000000000000000000, 1.000000000000000000, 0.000000000000000000 ) ) ;
#13832 = CARTESIAN_POINT ( 'NONE',  ( 190.0000000000000853, 15.53993994372673804, 38.07518420361041933 ) ) ;
#13833 = DIRECTION ( 'NONE',  ( -1.000000000000000000, -0.000000000000000000, -0.000000000000000000 ) ) ;
#13834 = CIRCLE ( 'NONE', #4766, 0.5000000000000004441 ) ;
#13835 = EDGE_CURVE ( 'NONE', #1269, #1785, #11500, .T. ) ;
#13836 = CIRCLE ( 'NONE', #7541, 3.500000000000003109 ) ;
#13837 = AXIS2_PLACEMENT_3D ( 'NONE', #6349, #1746, #4115 ) ;
#13838 = CARTESIAN_POINT ( 'NONE',  ( -63.50000000000002842, 17.53993994372674692, -17.50000000000002487 ) ) ;
#13839 = ORIENTED_EDGE ( 'NONE', *, *, #401, .T. ) ;
#13840 = DIRECTION ( 'NONE',  ( 0.8731965799097686221, -0.4873681696970814659, 0.000000000000000000 ) ) ;
#13841 = EDGE_CURVE ( 'NONE', #5504, #6805, #5745, .T. ) ;
#13842 = CARTESIAN_POINT ( 'NONE',  ( -185.3517468524019591, 137.0386009272039871, -0.4547266291960738172 ) ) ;
#13843 = DIRECTION ( 'NONE',  ( 0.000000000000000000, 0.000000000000000000, 1.000000000000000000 ) ) ;
#13844 = ORIENTED_EDGE ( 'NONE', *, *, #5883, .F. ) ;
#13845 = CARTESIAN_POINT ( 'NONE',  ( -225.5636091402884915, 143.1065995042388863, -0.5218507872395625746 ) ) ;
#13846 = CARTESIAN_POINT ( 'NONE',  ( 204.1803465669382547, 51.62486026858844212, 0.6453845751958426913 ) ) ;
#13847 = ORIENTED_EDGE ( 'NONE', *, *, #14251, .F. ) ;
#13848 = CIRCLE ( 'NONE', #7057, 1.000000000000000000 ) ;
#13849 = ADVANCED_FACE ( 'NONE', ( #2311, #5072 ), #9736, .F. ) ;
#13850 = EDGE_CURVE ( 'NONE', #4671, #2454, #11948, .T. ) ;
#13851 = AXIS2_PLACEMENT_3D ( 'NONE', #14206, #15464, #1975 ) ;
#13852 = CARTESIAN_POINT ( 'NONE',  ( 174.2293059057019775, 61.25683321636181233, 7.600000000000002309 ) ) ;
#13853 = CYLINDRICAL_SURFACE ( 'NONE', #12492, 0.5000000000000004441 ) ;
#13854 = DIRECTION ( 'NONE',  ( 3.965082230804130220E-16, 1.090924371466202084E-47, 1.000000000000000000 ) ) ;
#13855 = CIRCLE ( 'NONE', #7067, 0.5000000000000004441 ) ;
#13856 = AXIS2_PLACEMENT_3D ( 'NONE', #1043, #7141, #4672 ) ;
#13857 = AXIS2_PLACEMENT_3D ( 'NONE', #6317, #13478, #1400 ) ;
#13858 = FACE_OUTER_BOUND ( 'NONE', #1814, .T. ) ;
#13859 = VERTEX_POINT ( 'NONE', #3726 ) ;
#13860 = CIRCLE ( 'NONE', #10845, 6.299128011492294732 ) ;
#13861 = DIRECTION ( 'NONE',  ( 0.000000000000000000, 8.673617379884035472E-17, -1.000000000000000000 ) ) ;
#13862 = EDGE_CURVE ( 'NONE', #14293, #873, #9576, .T. ) ;
#13863 = ADVANCED_FACE ( 'NONE', ( #8553 ), #14530, .F. ) ;
#13864 = ADVANCED_FACE ( 'NONE', ( #2461 ), #14061, .T. ) ;
#13865 = CARTESIAN_POINT ( 'NONE',  ( -174.6331699355062028, 120.3494046152724763, 9.441255307061881652 ) ) ;
#13866 = DIRECTION ( 'NONE',  ( -0.000000000000000000, 1.000000000000000000, -0.000000000000000000 ) ) ;
#13867 = LINE ( 'NONE', #13621, #10852 ) ;
#13868 = ORIENTED_EDGE ( 'NONE', *, *, #13184, .T. ) ;
#13869 = PLANE ( 'NONE',  #6599 ) ;
#13870 = VERTEX_POINT ( 'NONE', #2549 ) ;
#13871 = VERTEX_POINT ( 'NONE', #2628 ) ;
#13872 = VECTOR ( 'NONE', #4045, 1000.000000000000000 ) ;
#13873 = CARTESIAN_POINT ( 'NONE',  ( -63.50000000000002842, -179.3753867012115961, -29.38864891670827362 ) ) ;
#13874 = DIRECTION ( 'NONE',  ( -0.000000000000000000, 1.000000000000000000, 0.000000000000000000 ) ) ;
#13875 = TOROIDAL_SURFACE ( 'NONE', #3788, 1.000000000000000000, 0.5000000000000000000 ) ;
#13876 = VECTOR ( 'NONE', #2586, 1000.000000000000000 ) ;
#13877 = CARTESIAN_POINT ( 'NONE',  ( -174.1990073215050643, 116.1278056868591904, 4.018260756276598400 ) ) ;
#13878 = DIRECTION ( 'NONE',  ( 0.000000000000000000, 0.000000000000000000, 1.000000000000000000 ) ) ;
#13879 = DIRECTION ( 'NONE',  ( 0.000000000000000000, 0.000000000000000000, -1.000000000000000000 ) ) ;
#13880 = EDGE_CURVE ( 'NONE', #12081, #13177, #7761, .T. ) ;
#13881 = CARTESIAN_POINT ( 'NONE',  ( -76.00000000000001421, -179.8058001507315566, -17.50000000000002487 ) ) ;
#13882 = DIRECTION ( 'NONE',  ( 1.000000000000000000, 0.000000000000000000, 0.000000000000000000 ) ) ;
#13883 = VECTOR ( 'NONE', #8487, 999.9999999999998863 ) ;
#13884 = LINE ( 'NONE', #2194, #7586 ) ;
#13885 = CARTESIAN_POINT ( 'NONE',  ( -222.8948771076028947, 147.8880518610581305, -2.733432078552652023 ) ) ;
#13886 = EDGE_LOOP ( 'NONE', ( #6373, #1270, #8663, #11123 ) ) ;
#13887 = CYLINDRICAL_SURFACE ( 'NONE', #2257, 1.700000000000007061 ) ;
#13888 = EDGE_LOOP ( 'NONE', ( #5918, #8419, #11000, #14534 ) ) ;
#13889 = CARTESIAN_POINT ( 'NONE',  ( -174.2806066667207858, 115.9816076509688401, 1.710173242044437991 ) ) ;
#13890 = CARTESIAN_POINT ( 'NONE',  ( 64.00000000000005684, 64.53993994372673626, 16.70000000000069207 ) ) ;
#13891 = DIRECTION ( 'NONE',  ( -0.000000000000000000, -0.000000000000000000, 1.000000000000000000 ) ) ;
#13892 = DIRECTION ( 'NONE',  ( -1.000000000000000000, 0.000000000000000000, -0.000000000000000000 ) ) ;
#13893 = CARTESIAN_POINT ( 'NONE',  ( -64.00000000000002842, 15.03993994372673981, -3.075184203610571654 ) ) ;
#13894 = AXIS2_PLACEMENT_3D ( 'NONE', #7213, #12952, #9649 ) ;
#13895 = ADVANCED_FACE ( 'NONE', ( #626 ), #11300, .F. ) ;
#13896 = CIRCLE ( 'NONE', #265, 4.172000000000013920 ) ;
#13897 = DIRECTION ( 'NONE',  ( 0.000000000000000000, 0.000000000000000000, 1.000000000000000000 ) ) ;
#13898 = ORIENTED_EDGE ( 'NONE', *, *, #1764, .F. ) ;
#13899 = SHAPE_DEFINITION_REPRESENTATION ( #9550, #10258 ) ;
#13900 = ORIENTED_EDGE ( 'NONE', *, *, #4649, .F. ) ;
#13901 = CARTESIAN_POINT ( 'NONE',  ( 203.9760488007458719, 51.69772753023573131, 0.6543994141905550288 ) ) ;
#13902 = LINE ( 'NONE', #8372, #4731 ) ;
#13903 = ORIENTED_EDGE ( 'NONE', *, *, #13436, .F. ) ;
#13904 = CARTESIAN_POINT ( 'NONE',  ( 164.0000000000000568, 62.13993994372673768, 15.00000000000000355 ) ) ;
#13905 = VECTOR ( 'NONE', #14423, 1000.000000000000000 ) ;
#13906 = DIRECTION ( 'NONE',  ( -0.000000000000000000, 1.000000000000000000, -0.000000000000000000 ) ) ;
#13907 = ORIENTED_EDGE ( 'NONE', *, *, #7733, .F. ) ;
#13908 = ORIENTED_EDGE ( 'NONE', *, *, #2798, .F. ) ;
#13909 = AXIS2_PLACEMENT_3D ( 'NONE', #13154, #2354, #4478 ) ;
#13910 = CARTESIAN_POINT ( 'NONE',  ( 190.5000000000000568, 19.53993994372674692, -17.50000000000002487 ) ) ;
#13911 = CARTESIAN_POINT ( 'NONE',  ( 178.0000000000000853, -179.3058001507315566, -30.31842631998718574 ) ) ;
#13912 = VERTEX_POINT ( 'NONE', #12475 ) ;
#13914 = EDGE_CURVE ( 'NONE', #9742, #6010, #6523, .T. ) ;
#13913 = CARTESIAN_POINT ( 'NONE',  ( 64.00000000000005684, 62.13993994372673768, 16.70000000000069207 ) ) ;
#13915 = CYLINDRICAL_SURFACE ( 'NONE', #750, 7.499999999999999112 ) ;
#13916 = DIRECTION ( 'NONE',  ( -0.000000000000000000, 1.000000000000000000, -0.000000000000000000 ) ) ;
#13917 = CYLINDRICAL_SURFACE ( 'NONE', #5957, 0.5000000000000004441 ) ;
#13918 = CARTESIAN_POINT ( 'NONE',  ( -81.74955057502458544, 65.19100426474074084, 10.00000000000000178 ) ) ;
#13919 = CIRCLE ( 'NONE', #286, 5.000000000000000000 ) ;
#13920 =( GEOMETRIC_REPRESENTATION_CONTEXT ( 3 ) GLOBAL_UNCERTAINTY_ASSIGNED_CONTEXT ( ( #8022 ) ) GLOBAL_UNIT_ASSIGNED_CONTEXT ( ( #12007, #13572, #9483 ) ) REPRESENTATION_CONTEXT ( 'NONE', 'WORKASPACE' ) );
#13921 = CARTESIAN_POINT ( 'NONE',  ( -76.50000000000001421, 16.03993994372673981, 10.05257423913146475 ) ) ;
#13922 = EDGE_LOOP ( 'NONE', ( #1320, #1421, #10206, #2780 ) ) ;
#13923 = ADVANCED_FACE ( 'NONE', ( #7847 ), #9021, .F. ) ;
#13924 = PLANE ( 'NONE',  #5429 ) ;
#13925 = CARTESIAN_POINT ( 'NONE',  ( -193.7157043470890301, 142.0697917816768836, 1.515441477536284332 ) ) ;
#13926 = CARTESIAN_POINT ( 'NONE',  ( -76.00000000000001421, -178.8058001507315566, -17.19066787724516843 ) ) ;
#13927 = ORIENTED_EDGE ( 'NONE', *, *, #13511, .T. ) ;
#13928 = CARTESIAN_POINT ( 'NONE',  ( -179.1950877003932874, 117.8811570380880909, -0.5844242688643165318 ) ) ;
#13929 = CARTESIAN_POINT ( 'NONE',  ( 190.7088546992480076, 48.18597428004899541, -1.751405883087224113 ) ) ;
#13930 = ORIENTED_EDGE ( 'NONE', *, *, #10623, .F. ) ;
#13932 = CIRCLE ( 'NONE', #10662, 3.500000000000001332 ) ;
#13931 = AXIS2_PLACEMENT_3D ( 'NONE', #5143, #2937, #11224 ) ;
#13933 = DIRECTION ( 'NONE',  ( 0.000000000000000000, -0.1391731009600592484, 0.9902680687415712502 ) ) ;
#13934 = DIRECTION ( 'NONE',  ( -0.000000000000000000, 1.000000000000000000, -0.000000000000000000 ) ) ;
#13935 = CARTESIAN_POINT ( 'NONE',  ( 178.0000000000000853, 15.17911304468679745, 25.93769382960995529 ) ) ;
#13936 = ADVANCED_FACE ( 'NONE', ( #4182 ), #2785, .T. ) ;
#13937 =( NAMED_UNIT ( * ) PLANE_ANGLE_UNIT ( ) SI_UNIT ( $, .RADIAN. ) );
#13938 = DIRECTION ( 'NONE',  ( 8.659560562354932858E-17, 0.7071067811865474617, -0.7071067811865474617 ) ) ;
#13939 = ORIENTED_EDGE ( 'NONE', *, *, #3168, .F. ) ;
#13940 = DIRECTION ( 'NONE',  ( 0.000000000000000000, 1.000000000000000000, 8.673617379884035472E-17 ) ) ;
#13941 = CARTESIAN_POINT ( 'NONE',  ( -223.5464781713420734, 146.7206062712571111, 9.530069280832668355 ) ) ;
#13942 = CYLINDRICAL_SURFACE ( 'NONE', #13557, 1.699999999999994849 ) ;
#13943 = DIRECTION ( 'NONE',  ( 0.000000000000000000, -0.5000000000000012212, -0.8660254037844380415 ) ) ;
#13944 = PRODUCT ( 'Long Manual Lever Operating Handle', 'Long Manual Lever Operating Handle', '', ( #3092 ) ) ;
#13945 = ORIENTED_EDGE ( 'NONE', *, *, #5482, .F. ) ;
#13946 = DIRECTION ( 'NONE',  ( 0.000000000000000000, 0.000000000000000000, -1.000000000000000000 ) ) ;
#13947 = AXIS2_PLACEMENT_3D ( 'NONE', #670, #2755, #1640 ) ;
#13948 = ORIENTED_EDGE ( 'NONE', *, *, #14264, .T. ) ;
#13949 = VERTEX_POINT ( 'NONE', #1742 ) ;
#13950 = CARTESIAN_POINT ( 'NONE',  ( -152.4086188282879561, 107.4000165207912261, 9.455162786586091883 ) ) ;
#13951 = LINE ( 'NONE', #6708, #11051 ) ;
#13952 = CARTESIAN_POINT ( 'NONE',  ( 17.41029453487719181, 40.04259805664093363, 10.00000000000000178 ) ) ;
#13953 = CARTESIAN_POINT ( 'NONE',  ( -173.8627125986912176, 116.7303304721469885, 5.982824555829307833 ) ) ;
#13954 = CARTESIAN_POINT ( 'NONE',  ( -219.3428653954115646, 154.2520384152134625, -2.513716752921474118 ) ) ;
#13955 = CIRCLE ( 'NONE', #13195, 1.499999999999995115 ) ;
#13956 = EDGE_CURVE ( 'NONE', #10772, #4850, #3720, .T. ) ;
#13958 = EDGE_CURVE ( 'NONE', #8697, #8310, #7015, .T. ) ;
#13957 = EDGE_CURVE ( 'NONE', #13797, #11925, #12533, .T. ) ;
#13959 = CARTESIAN_POINT ( 'NONE',  ( 19.11029453487719110, 40.04259805664093363, 10.00000000000000178 ) ) ;
#13960 = VECTOR ( 'NONE', #7739, 1000.000000000000000 ) ;
#13961 = DIRECTION ( 'NONE',  ( 0.000000000000000000, 0.000000000000000000, 1.000000000000000000 ) ) ;
#13962 = DIRECTION ( 'NONE',  ( 0.000000000000000000, 0.8660254037844388186, 0.4999999999999996669 ) ) ;
#13963 = FACE_OUTER_BOUND ( 'NONE', #2510, .T. ) ;
#13964 = CARTESIAN_POINT ( 'NONE',  ( -220.8828325426286767, 151.4929455369283176, -2.526440127944020286 ) ) ;
#13965 = VERTEX_POINT ( 'NONE', #7609 ) ;
#13966 = CIRCLE ( 'NONE', #8930, 1.700000000000007061 ) ;
#13967 = ORIENTED_EDGE ( 'NONE', *, *, #4482, .F. ) ;
#13968 = DIRECTION ( 'NONE',  ( -0.000000000000000000, -0.000000000000000000, 1.000000000000000000 ) ) ;
#13969 = CYLINDRICAL_SURFACE ( 'NONE', #9886, 0.5000000000000004441 ) ;
#13971 = DIRECTION ( 'NONE',  ( 0.000000000000000000, 0.000000000000000000, -1.000000000000000000 ) ) ;
#13970 = VECTOR ( 'NONE', #6455, 1000.000000000000000 ) ;
#13972 = CARTESIAN_POINT ( 'NONE',  ( 190.0000000000000568, 16.03993994372673981, -7.458121719691109004E-14 ) ) ;
#13973 = CARTESIAN_POINT ( 'NONE',  ( 5.799999999999999822, -9.237604307034018802, 2.775557561562891351E-14 ) ) ;
#13974 = DIRECTION ( 'NONE',  ( 0.000000000000000000, 0.000000000000000000, 1.000000000000000000 ) ) ;
#13975 = ORIENTED_EDGE ( 'NONE', *, *, #6277, .T. ) ;
#13976 =( GEOMETRIC_REPRESENTATION_CONTEXT ( 3 ) GLOBAL_UNCERTAINTY_ASSIGNED_CONTEXT ( ( #11796 ) ) GLOBAL_UNIT_ASSIGNED_CONTEXT ( ( #4919, #3724, #307 ) ) REPRESENTATION_CONTEXT ( 'NONE', 'WORKASPACE' ) );
#13977 = ITEM_DEFINED_TRANSFORMATION ( 'NONE', 'NONE', #15585,  #12337 ) ;
#13978 = ORIENTED_EDGE ( 'NONE', *, *, #10517, .F. ) ;
#13979 = CARTESIAN_POINT ( 'NONE',  ( 190.6221111713484788, 48.05726534264031358, -4.889407597981446862 ) ) ;
#13980 = EDGE_LOOP ( 'NONE', ( #2104, #13586 ) ) ;
#13981 = DIRECTION ( 'NONE',  ( 0.000000000000000000, 0.000000000000000000, 1.000000000000000000 ) ) ;
#13982 = CARTESIAN_POINT ( 'NONE',  ( -164.5262273476079713, 106.7842295329138835, 5.000000000000000000 ) ) ;
#13983 = ORIENTED_EDGE ( 'NONE', *, *, #10730, .F. ) ;
#13984 = ORIENTED_EDGE ( 'NONE', *, *, #13378, .F. ) ;
#13985 = DIRECTION ( 'NONE',  ( -0.000000000000000000, -0.000000000000000000, 1.000000000000000000 ) ) ;
#13986 = ADVANCED_FACE ( 'NONE', ( #9976 ), #10046, .F. ) ;
#13987 = AXIS2_PLACEMENT_3D ( 'NONE', #15031, #7958, #6620 ) ;
#13988 = VERTEX_POINT ( 'NONE', #545 ) ;
#13989 = CARTESIAN_POINT ( 'NONE',  ( 191.3918663844754349, 39.68659111044760124, -5.934329888686073140 ) ) ;
#13990 = DIRECTION ( 'NONE',  ( -0.4873681696970814659, -0.8731965799097686221, 0.000000000000000000 ) ) ;
#13991 = CARTESIAN_POINT ( 'NONE',  ( 169.0293059057019889, 61.25683321636181233, 7.600000000000002309 ) ) ;
#13992 = DIRECTION ( 'NONE',  ( 0.8731965799097682890, -0.4873681696970819099, -0.000000000000000000 ) ) ;
#13993 = CYLINDRICAL_SURFACE ( 'NONE', #8340, 1.499999999999994449 ) ;
#13994 = LINE ( 'NONE', #3182, #1500 ) ;
#13995 = ORIENTED_EDGE ( 'NONE', *, *, #15050, .T. ) ;
#13996 = DIRECTION ( 'NONE',  ( 1.000000000000000000, 0.000000000000000000, 0.000000000000000000 ) ) ;
#13997 = CARTESIAN_POINT ( 'NONE',  ( -198.7485669925355012, 144.4350871509360559, -0.4547266291960735951 ) ) ;
#13998 = CARTESIAN_POINT ( 'NONE',  ( 203.4093511297053851, 50.30250970312692971, -0.9107274384406970347 ) ) ;
#13999 = VERTEX_POINT ( 'NONE', #2704 ) ;
#14000 = EDGE_CURVE ( 'NONE', #11935, #10092, #12634, .T. ) ;
#14001 = CARTESIAN_POINT ( 'NONE',  ( -173.2784152866543934, 122.7799518889917465, -5.329639836781006501 ) ) ;
#14002 = CARTESIAN_POINT ( 'NONE',  ( 192.9750851430037528, 31.35397111148814631, -7.136603044727629630 ) ) ;
#14003 = ORIENTED_EDGE ( 'NONE', *, *, #1163, .T. ) ;
#14004 = AXIS2_PLACEMENT_3D ( 'NONE', #10356, #15151, #10277 ) ;
#14005 = LINE ( 'NONE', #8025, #6412 ) ;
#14006 = DIRECTION ( 'NONE',  ( -3.965082230804130220E-16, 1.090924371466202084E-47, 1.000000000000000000 ) ) ;
#14007 = FACE_OUTER_BOUND ( 'NONE', #14545, .T. ) ;
#14008 = VERTEX_POINT ( 'NONE', #3887 ) ;
#14009 = FACE_OUTER_BOUND ( 'NONE', #8163, .T. ) ;
#14010 = ORIENTED_EDGE ( 'NONE', *, *, #8288, .F. ) ;
#14011 = DIRECTION ( 'NONE',  ( -0.000000000000000000, 0.9902680687415712502, 0.1391731009600584990 ) ) ;
#14012 = CARTESIAN_POINT ( 'NONE',  ( -190.6501653245252044, 127.3085702864440520, 7.918248976830637886 ) ) ;
#14013 = DIRECTION ( 'NONE',  ( 0.000000000000000000, 0.000000000000000000, -1.000000000000000000 ) ) ;
#14014 = FACE_OUTER_BOUND ( 'NONE', #12892, .T. ) ;
#14015 = ORIENTED_EDGE ( 'NONE', *, *, #10533, .F. ) ;
#14016 = CARTESIAN_POINT ( 'NONE',  ( 6.399999999999999467, 9.237604307034018802, 0.000000000000000000 ) ) ;
#14017 = CIRCLE ( 'NONE', #7992, 1.700000000000007061 ) ;
#14018 = EDGE_CURVE ( 'NONE', #9103, #5262, #11696, .T. ) ;
#14019 = ORIENTED_EDGE ( 'NONE', *, *, #7900, .F. ) ;
#14020 = EDGE_LOOP ( 'NONE', ( #5414, #14219, #10854, #9222 ) ) ;
#14021 = DIRECTION ( 'NONE',  ( 0.000000000000000000, 0.000000000000000000, 1.000000000000000000 ) ) ;
#14022 = DIRECTION ( 'NONE',  ( 1.000000000000000000, 0.000000000000000000, 0.000000000000000000 ) ) ;
#14023 = CARTESIAN_POINT ( 'NONE',  ( 5.799999999999999822, -9.237604307034018802, 2.775557561562891351E-14 ) ) ;
#14024 = PLANE ( 'NONE',  #6242 ) ;
#14025 = CARTESIAN_POINT ( 'NONE',  ( -223.7640232666028623, 146.3308400842772130, -1.599190326327902367 ) ) ;
#14026 = DIRECTION ( 'NONE',  ( -0.8731965799097684000, 0.4873681696970815769, 0.000000000000000000 ) ) ;
#14027 = AXIS2_PLACEMENT_3D ( 'NONE', #9872, #11046, #11204 ) ;
#14028 = FACE_OUTER_BOUND ( 'NONE', #5765, .T. ) ;
#14029 = CARTESIAN_POINT ( 'NONE',  ( 190.0000000000000568, -178.8058001507315566, -17.19066787724516843 ) ) ;
#14030 = EDGE_CURVE ( 'NONE', #13094, #14396, #1698, .T. ) ;
#14031 = CARTESIAN_POINT ( 'NONE',  ( 177.5000000000000853, -178.8058001507315566, -17.19066787724516843 ) ) ;
#14032 = LINE ( 'NONE', #6871, #6067 ) ;
#14033 = CARTESIAN_POINT ( 'NONE',  ( -224.3206423883182765, 145.3335695532608440, -0.03206942370135386355 ) ) ;
#14034 = ORIENTED_EDGE ( 'NONE', *, *, #6558, .T. ) ;
#14035 =( NAMED_UNIT ( * ) PLANE_ANGLE_UNIT ( ) SI_UNIT ( $, .RADIAN. ) );
#14036 = PRODUCT_DEFINITION ( 'UNKNOWN', '', #6531, #1872 ) ;
#14037 = ORIENTED_EDGE ( 'NONE', *, *, #10572, .F. ) ;
#14038 = CARTESIAN_POINT ( 'NONE',  ( -150.4086188282879277, 107.2728346664360259, 84.88378295107887084 ) ) ;
#14039 = CARTESIAN_POINT ( 'NONE',  ( -135.3034657297974093, 107.4444500778096483, 0.000000000000000000 ) ) ;
#14040 = CARTESIAN_POINT ( 'NONE',  ( -110.0000000000000426, 19.53993994372674337, 9.999999999999998224 ) ) ;
#14041 = CYLINDRICAL_SURFACE ( 'NONE', #5815, 0.5000000000000004441 ) ;
#14042 = EDGE_CURVE ( 'NONE', #13140, #5266, #9782, .T. ) ;
#14043 = DIRECTION ( 'NONE',  ( -0.000000000000000000, 0.9902680687415702510, 0.1391731009600660485 ) ) ;
#14044 = ORIENTED_EDGE ( 'NONE', *, *, #8531, .T. ) ;
#14045 = CONTEXT_DEPENDENT_SHAPE_REPRESENTATION ( #6166, #15061 ) ;
#14046 = VERTEX_POINT ( 'NONE', #10725 ) ;
#14047 = CARTESIAN_POINT ( 'NONE',  ( 201.5861714792528119, 52.66925088518574682, -5.382215963875594866 ) ) ;
#14048 = VERTEX_POINT ( 'NONE', #3384 ) ;
#14049 = DIRECTION ( 'NONE',  ( -0.000000000000000000, -0.000000000000000000, 1.000000000000000000 ) ) ;
#14050 = EDGE_CURVE ( 'NONE', #14894, #10019, #13902, .T. ) ;
#14051 = ADVANCED_FACE ( 'NONE', ( #3615 ), #1953, .F. ) ;
#14052 = CARTESIAN_POINT ( 'NONE',  ( -223.5992072901615018, 142.0487386537765246, 3.276137811062253213 ) ) ;
#14053 = ORIENTED_EDGE ( 'NONE', *, *, #1947, .T. ) ;
#14054 = ORIENTED_EDGE ( 'NONE', *, *, #9637, .F. ) ;
#14055 = CYLINDRICAL_SURFACE ( 'NONE', #7540, 5.000000000000017764 ) ;
#14056 = FACE_BOUND ( 'NONE', #10115, .T. ) ;
#14057 = ORIENTED_EDGE ( 'NONE', *, *, #4687, .T. ) ;
#14058 = VECTOR ( 'NONE', #669, 1000.000000000000000 ) ;
#14059 = DIRECTION ( 'NONE',  ( 0.000000000000000000, 0.000000000000000000, -1.000000000000000000 ) ) ;
#14060 = DIRECTION ( 'NONE',  ( -0.4873681696970814659, -0.8731965799097686221, 0.000000000000000000 ) ) ;
#14061 = TOROIDAL_SURFACE ( 'NONE', #2471, 1.000000000000000000, 0.5000000000000000000 ) ;
#14062 = DIRECTION ( 'NONE',  ( 0.000000000000000000, 1.000000000000000000, 6.938893903907227145E-17 ) ) ;
#14063 = DIRECTION ( 'NONE',  ( -0.000000000000000000, 1.000000000000000000, 6.938893903907227145E-17 ) ) ;
#14064 = LINE ( 'NONE', #877, #478 ) ;
#14065 = PRODUCT_DEFINITION_SHAPE ( 'NONE', 'NONE',  #15632 ) ;
#14066 = EDGE_CURVE ( 'NONE', #6010, #11247, #9102, .T. ) ;
#14067 = DIRECTION ( 'NONE',  ( -1.000000000000000000, 0.000000000000000000, 0.000000000000000000 ) ) ;
#14068 = AXIS2_PLACEMENT_3D ( 'NONE', #2783, #13129, #7603 ) ;
#14069 = ORIENTED_EDGE ( 'NONE', *, *, #967, .T. ) ;
#14070 = FACE_BOUND ( 'NONE', #7508, .T. ) ;
#14071 = CONICAL_SURFACE ( 'NONE', #5754, 3.525000000000000355, 0.7853981633975176679 ) ;
#14072 = CARTESIAN_POINT ( 'NONE',  ( -212.2154691228631691, 150.1790628786027355, -2.963320117457098224 ) ) ;
#14073 = CARTESIAN_POINT ( 'NONE',  ( 184.0000000000000568, 17.53993994372673981, -13.99999999999999289 ) ) ;
#14074 = ORIENTED_EDGE ( 'NONE', *, *, #12208, .F. ) ;
#14075 = CARTESIAN_POINT ( 'NONE',  ( -199.2233958860587961, 127.9753750774359276, -0.4555467707853375070 ) ) ;
#14076 = CARTESIAN_POINT ( 'NONE',  ( 202.9867918041427686, 48.86553571320913392, 0.6621522355815065985 ) ) ;
#14077 = ORIENTED_EDGE ( 'NONE', *, *, #14081, .F. ) ;
#14078 = DIRECTION ( 'NONE',  ( 1.000000000000000000, 0.000000000000000000, 0.000000000000000000 ) ) ;
#14079 = FACE_OUTER_BOUND ( 'NONE', #5194, .T. ) ;
#14080 = PLANE ( 'NONE',  #9064 ) ;
#14081 = EDGE_CURVE ( 'NONE', #9280, #4290, #10042, .T. ) ;
#14082 = ORIENTED_EDGE ( 'NONE', *, *, #9905, .F. ) ;
#14083 = DIRECTION ( 'NONE',  ( 0.000000000000000000, 0.000000000000000000, 1.000000000000000000 ) ) ;
#14084 = DIRECTION ( 'NONE',  ( 5.518327896226369609E-17, -0.9902680687415712502, -0.1391731009600584990 ) ) ;
#14085 = EDGE_LOOP ( 'NONE', ( #3888, #3294, #3291, #2058 ) ) ;
#14086 = DIRECTION ( 'NONE',  ( -0.000000000000000000, 1.000000000000000000, -0.000000000000000000 ) ) ;
#14087 = CARTESIAN_POINT ( 'NONE',  ( -187.1267843490969369, 133.7770572797440991, 9.578254705571838556 ) ) ;
#14088 = AXIS2_PLACEMENT_3D ( 'NONE', #13750, #2799, #11241 ) ;
#14089 = DIRECTION ( 'NONE',  ( 3.965082230804130220E-16, -4.956352788505162775E-17, 1.000000000000000000 ) ) ;
#14090 = CARTESIAN_POINT ( 'NONE',  ( 164.0000000000000568, 64.53993994372673626, 15.00000000000000355 ) ) ;
#14091 = VERTEX_POINT ( 'NONE', #2353 ) ;
#14092 = LINE ( 'NONE', #11668, #6845 ) ;
#14093 = CIRCLE ( 'NONE', #464, 1.699999999999993072 ) ;
#14094 = ORIENTED_EDGE ( 'NONE', *, *, #917, .F. ) ;
#14095 = VERTEX_POINT ( 'NONE', #13231 ) ;
#14096 = DIRECTION ( 'NONE',  ( 0.000000000000000000, 0.000000000000000000, 1.000000000000000000 ) ) ;
#14097 = CARTESIAN_POINT ( 'NONE',  ( 164.0000000000000568, 59.53993994372674337, 16.70000000000000995 ) ) ;
#14098 = FACE_OUTER_BOUND ( 'NONE', #2226, .T. ) ;
#14099 = CARTESIAN_POINT ( 'NONE',  ( -174.2675151123989110, 116.0050632255638163, 3.108104069861567620 ) ) ;
#14100 = AXIS2_PLACEMENT_3D ( 'NONE', #503, #5344, #8909 ) ;
#14101 = CARTESIAN_POINT ( 'NONE',  ( -220.0780021574012721, 148.8225603397216901, -5.061978238651692941 ) ) ;
#14102 = CARTESIAN_POINT ( 'NONE',  ( -70.00000000000000000, -179.3058001507315566, -41.45141194869120227 ) ) ;
#14103 = CARTESIAN_POINT ( 'NONE',  ( 178.0000000000000853, -178.8058001507315566, -30.31842631998718574 ) ) ;
#14104 = FACE_OUTER_BOUND ( 'NONE', #9185, .T. ) ;
#14105 = ADVANCED_FACE ( 'NONE', ( #9388 ), #2209, .T. ) ;
#14106 = LINE ( 'NONE', #9164, #5668 ) ;
#14107 = DIRECTION ( 'NONE',  ( 0.000000000000000000, 0.000000000000000000, 1.000000000000000000 ) ) ;
#14108 = VECTOR ( 'NONE', #2538, 1000.000000000000000 ) ;
#14109 = CARTESIAN_POINT ( 'NONE',  ( -64.00000000000002842, 15.53993994372673981, -2.500000000000070610 ) ) ;
#14110 = ORIENTED_EDGE ( 'NONE', *, *, #8947, .T. ) ;
#14111 = EDGE_CURVE ( 'NONE', #8731, #899, #1443, .T. ) ;
#14112 = VECTOR ( 'NONE', #11476, 1000.000000000000000 ) ;
#14113 = VECTOR ( 'NONE', #1455, 1000.000000000000000 ) ;
#14114 = DIRECTION ( 'NONE',  ( -0.000000000000000000, -0.000000000000000000, 1.000000000000000000 ) ) ;
#14115 = ORIENTED_EDGE ( 'NONE', *, *, #2051, .T. ) ;
#14116 = CARTESIAN_POINT ( 'NONE',  ( -76.00000000000001421, 15.03993994372673981, -3.075184203610571654 ) ) ;
#14117 = CARTESIAN_POINT ( 'NONE',  ( 64.00000000000005684, 62.13993994372673768, 15.00000000000070166 ) ) ;
#14118 = ORIENTED_EDGE ( 'NONE', *, *, #8412, .T. ) ;
#14119 = CARTESIAN_POINT ( 'NONE',  ( -164.5262273476079713, 106.7842295329138835, 5.000000000000000000 ) ) ;
#14120 = DIRECTION ( 'NONE',  ( 1.000000000000000000, 0.000000000000000000, 3.965082230804112963E-16 ) ) ;
#14121 = VECTOR ( 'NONE', #6181, 1000.000000000000000 ) ;
#14122 = DIRECTION ( 'NONE',  ( 0.000000000000000000, 0.000000000000000000, -1.000000000000000000 ) ) ;
#14123 = EDGE_LOOP ( 'NONE', ( #7551, #2853, #1747, #13077 ) ) ;
#14124 = VECTOR ( 'NONE', #5714, 1000.000000000000000 ) ;
#14125 = ADVANCED_FACE ( 'NONE', ( #7190 ), #2272, .T. ) ;
#14126 = VECTOR ( 'NONE', #4375, 1000.000000000000000 ) ;
#14127 = EDGE_LOOP ( 'NONE', ( #13801, #118, #12485, #5920 ) ) ;
#14128 = DIRECTION ( 'NONE',  ( 0.000000000000000000, 0.000000000000000000, -1.000000000000000000 ) ) ;
#14129 = EDGE_LOOP ( 'NONE', ( #5076, #5838, #11897, #11448 ) ) ;
#14130 = CARTESIAN_POINT ( 'NONE',  ( 6.399999999999999467, 9.237604307034018802, 0.000000000000000000 ) ) ;
#14131 = DIRECTION ( 'NONE',  ( 0.000000000000000000, 4.956352788505162775E-17, -1.000000000000000000 ) ) ;
#14132 = CARTESIAN_POINT ( 'NONE',  ( 178.0000000000000853, 15.03993994372673981, 10.05257423913146475 ) ) ;
#14133 = CIRCLE ( 'NONE', #1272, 1.500000000000000000 ) ;
#14134 = ORIENTED_EDGE ( 'NONE', *, *, #13363, .F. ) ;
#14135 = ORIENTED_EDGE ( 'NONE', *, *, #624, .T. ) ;
#14136 = DIRECTION ( 'NONE',  ( -0.000000000000000000, -0.9902680687415710281, 0.1391731009600611635 ) ) ;
#14137 = DIRECTION ( 'NONE',  ( 0.000000000000000000, -1.000000000000000000, 0.000000000000000000 ) ) ;
#14138 = AXIS2_PLACEMENT_3D ( 'NONE', #3292, #15344, #3206 ) ;
#14139 = ORIENTED_EDGE ( 'NONE', *, *, #15238, .T. ) ;
#14140 = DIRECTION ( 'NONE',  ( -1.000000000000000000, 0.000000000000000000, 3.965082230804112963E-16 ) ) ;
#14141 = DIRECTION ( 'NONE',  ( 0.000000000000000000, 0.000000000000000000, 1.000000000000000000 ) ) ;
#14142 = CYLINDRICAL_SURFACE ( 'NONE', #8821, 17.06579782980005433 ) ;
#14143 = EDGE_CURVE ( 'NONE', #4926, #7373, #5908, .T. ) ;
#14144 = EDGE_CURVE ( 'NONE', #4933, #5606, #15236, .T. ) ;
#14145 = EDGE_CURVE ( 'NONE', #13250, #6618, #5242, .T. ) ;
#14146 = VECTOR ( 'NONE', #4020, 1000.000000000000000 ) ;
#14147 = DIRECTION ( 'NONE',  ( 0.000000000000000000, 0.000000000000000000, 1.000000000000000000 ) ) ;
#14148 = VECTOR ( 'NONE', #23, 1000.000000000000000 ) ;
#14149 = ORIENTED_EDGE ( 'NONE', *, *, #6717, .F. ) ;
#14150 = LINE ( 'NONE', #6026, #5689 ) ;
#14151 = CARTESIAN_POINT ( 'NONE',  ( -215.1139964504661464, 145.4140256597743814, 2.431557144026069928 ) ) ;
#14152 = CARTESIAN_POINT ( 'NONE',  ( -110.0000000000000426, 59.53993994372674337, 25.00000000000000000 ) ) ;
#14153 = ORIENTED_EDGE ( 'NONE', *, *, #10427, .F. ) ;
#14154 = CARTESIAN_POINT ( 'NONE',  ( -186.4817914481332366, 122.8418524018552063, -2.964974570226826867 ) ) ;
#14155 = CARTESIAN_POINT ( 'NONE',  ( 203.9349922441545857, 30.00251698353133989, -9.664403529890410738 ) ) ;
#14156 = EDGE_LOOP ( 'NONE', ( #9554, #2727 ) ) ;
#14157 = VECTOR ( 'NONE', #14952, 1000.000000000000000 ) ;
#14158 = CYLINDRICAL_SURFACE ( 'NONE', #9320, 0.5000000000000004441 ) ;
#14159 = CARTESIAN_POINT ( 'NONE',  ( 0.000000000000000000, 7.511572993685799101E-16, -2.750000000000000444 ) ) ;
#14160 = CARTESIAN_POINT ( 'NONE',  ( -83.77455057502459113, 65.19100426474074084, 5.000000000000000000 ) ) ;
#14161 = ORIENTED_EDGE ( 'NONE', *, *, #15290, .F. ) ;
#14162 = CARTESIAN_POINT ( 'NONE',  ( 14.00000000000004086, 59.53993994372674337, 16.70000000000105089 ) ) ;
#14163 = CARTESIAN_POINT ( 'NONE',  ( 207.1194509196011495, 46.14302886020001182, -1.185720282267065828 ) ) ;
#14164 = EDGE_LOOP ( 'NONE', ( #10527, #7446, #14733, #3273 ) ) ;
#14165 = CIRCLE ( 'NONE', #8152, 54.67486482576605766 ) ;
#14166 = DIRECTION ( 'NONE',  ( 1.000000000000000000, 0.000000000000000000, -0.000000000000000000 ) ) ;
#14167 = CARTESIAN_POINT ( 'NONE',  ( -179.3772030532177837, 117.5545944912402661, 3.345861034185851235 ) ) ;
#14168 = DIRECTION ( 'NONE',  ( -0.000000000000000000, 0.000000000000000000, 1.000000000000000000 ) ) ;
#14169 = CARTESIAN_POINT ( 'NONE',  ( 152.8671246545933400, 7.480744990243093362, -7.157132912367466737 ) ) ;
#14170 = CARTESIAN_POINT ( 'NONE',  ( 184.0000000000000568, -179.3058001507315566, -39.95141194869120937 ) ) ;
#14171 = VERTEX_POINT ( 'NONE', #7104 ) ;
#14172 = EDGE_LOOP ( 'NONE', ( #14538, #4781, #2245, #11602, #11273, #2546, #14303, #6652, #10261 ) ) ;
#14173 = CARTESIAN_POINT ( 'NONE',  ( 5.196152422706635576, -9.000000000000003553, 5.000000000000000000 ) ) ;
#14174 = DIRECTION ( 'NONE',  ( 1.000000000000000000, 0.000000000000000000, 0.000000000000000000 ) ) ;
#14175 = EDGE_CURVE ( 'NONE', #411, #6899, #4480, .T. ) ;
#14176 = DIRECTION ( 'NONE',  ( -0.000000000000000000, -1.000000000000000000, -0.000000000000000000 ) ) ;
#14177 = DIRECTION ( 'NONE',  ( -0.000000000000000000, -0.000000000000000000, 1.000000000000000000 ) ) ;
#14178 = CARTESIAN_POINT ( 'NONE',  ( -222.4732244369151886, 144.2379617518073474, -3.208335888254660428 ) ) ;
#14179 = CARTESIAN_POINT ( 'NONE',  ( 21.99999999999999289, 0.000000000000000000, 0.000000000000000000 ) ) ;
#14180 = CONICAL_SURFACE ( 'NONE', #3850, 3.525000000000000355, 0.7853981633973787790 ) ;
#14181 = FACE_OUTER_BOUND ( 'NONE', #14020, .T. ) ;
#14182 = CARTESIAN_POINT ( 'NONE',  ( 190.0000000000000568, -178.9449732516916072, -29.32815825124561471 ) ) ;
#14183 = CIRCLE ( 'NONE', #3634, 1.499999999999994227 ) ;
#14184 = CARTESIAN_POINT ( 'NONE',  ( 0.000000000000000000, 0.000000000000000000, 5.000000000000000000 ) ) ;
#14185 = DIRECTION ( 'NONE',  ( -0.000000000000000000, 1.000000000000000000, -0.000000000000000000 ) ) ;
#14186 = DIRECTION ( 'NONE',  ( -0.8950274278067241740, 0.4460111024107797362, -0.000000000000000000 ) ) ;
#14187 = VERTEX_POINT ( 'NONE', #4801 ) ;
#14188 = DIRECTION ( 'NONE',  ( 1.000000000000000000, 0.000000000000000000, 0.000000000000000000 ) ) ;
#14189 = ORIENTED_EDGE ( 'NONE', *, *, #5457, .T. ) ;
#14190 = EDGE_CURVE ( 'NONE', #4326, #13434, #14340, .T. ) ;
#14191 = CARTESIAN_POINT ( 'NONE',  ( 177.5000000000000853, 15.53993994372673981, -3.075184203610571654 ) ) ;
#14192 = DIRECTION ( 'NONE',  ( 0.000000000000000000, 0.000000000000000000, 1.000000000000000000 ) ) ;
#14193 = CIRCLE ( 'NONE', #7413, 2.000000000000000000 ) ;
#14194 = CARTESIAN_POINT ( 'NONE',  ( 0.06809871960542948632, -7.710219529346599820, 2.645508037661917555 ) ) ;
#14195 = CARTESIAN_POINT ( 'NONE',  ( 167.9295236634097819, 65.51901744756736434, -0.9107274384406985890 ) ) ;
#14196 = DIRECTION ( 'NONE',  ( -0.000000000000000000, 1.000000000000000000, -0.000000000000000000 ) ) ;
#14197 = AXIS2_PLACEMENT_3D ( 'NONE', #7817, #7657, #6473 ) ;
#14199 = VERTEX_POINT ( 'NONE', #10569 ) ;
#14198 = ADVANCED_FACE ( 'NONE', ( #5751, #7262 ), #12707, .T. ) ;
#14200 = ORIENTED_EDGE ( 'NONE', *, *, #10489, .F. ) ;
#14201 = AXIS2_PLACEMENT_3D ( 'NONE', #15437, #13227, #14489 ) ;
#14202 = CARTESIAN_POINT ( 'NONE',  ( 211.8802283582561472, 39.29745248741442509, -3.136047433260559902 ) ) ;
#14203 = CARTESIAN_POINT ( 'NONE',  ( 5.196152422706632024, 9.000000000000003553, 0.000000000000000000 ) ) ;
#14204 = VERTEX_POINT ( 'NONE', #15362 ) ;
#14205 = FACE_OUTER_BOUND ( 'NONE', #3638, .T. ) ;
#14206 = CARTESIAN_POINT ( 'NONE',  ( -76.00000000000004263, 16.03993994372673626, 38.07518420361041933 ) ) ;
#14207 = VERTEX_POINT ( 'NONE', #4564 ) ;
#14208 = ORIENTED_EDGE ( 'NONE', *, *, #13117, .F. ) ;
#14209 = DIRECTION ( 'NONE',  ( -0.000000000000000000, -0.000000000000000000, -1.000000000000000000 ) ) ;
#14210 = CARTESIAN_POINT ( 'NONE',  ( 191.8042410000843745, 59.95507574834591225, 0.000000000000000000 ) ) ;
#14211 = B_SPLINE_CURVE_WITH_KNOTS ( 'NONE', 3,
 ( #13207, #10703, #11966, #3665, #4616, #2405, #12978, #2247 ),
 .UNSPECIFIED., .F., .F.,
 ( 4, 2, 2, 4 ),
 ( 0.004673709593152154847, 0.005837709341827654677, 0.007001709090503155375, 0.009329708587854153301 ),
 .UNSPECIFIED. ) ;
#14212 = EDGE_CURVE ( 'NONE', #7455, #2394, #8792, .T. ) ;
#14213 = ORIENTED_EDGE ( 'NONE', *, *, #15381, .F. ) ;
#14214 = FACE_OUTER_BOUND ( 'NONE', #8700, .T. ) ;
#14215 = VECTOR ( 'NONE', #8220, 1000.000000000000000 ) ;
#14216 = DIRECTION ( 'NONE',  ( 0.000000000000000000, 0.000000000000000000, 1.000000000000000000 ) ) ;
#14217 = VECTOR ( 'NONE', #12393, 1000.000000000000114 ) ;
#14218 = EDGE_CURVE ( 'NONE', #6739, #10201, #1550, .T. ) ;
#14219 = ORIENTED_EDGE ( 'NONE', *, *, #10958, .F. ) ;
#14220 = LINE ( 'NONE', #3417, #6564 ) ;
#14221 = ORIENTED_EDGE ( 'NONE', *, *, #13234, .T. ) ;
#14222 = ADVANCED_FACE ( 'NONE', ( #8824 ), #3991, .F. ) ;
#14223 = DIRECTION ( 'NONE',  ( 0.000000000000000000, 1.000000000000000000, 6.938893903907227145E-17 ) ) ;
#14224 = AXIS2_PLACEMENT_3D ( 'NONE', #10084, #7646, #1383 ) ;
#14225 = DIRECTION ( 'NONE',  ( 0.05375305303998870188, 0.09630703232712070627, -0.9938991723576509063 ) ) ;
#14226 = DIRECTION ( 'NONE',  ( -0.000000000000000000, 0.000000000000000000, 1.000000000000000000 ) ) ;
#14227 = ORIENTED_EDGE ( 'NONE', *, *, #3577, .T. ) ;
#14228 = CARTESIAN_POINT ( 'NONE',  ( -208.3893201713671033, 134.8533518211819739, -2.964974570226836192 ) ) ;
#14229 = CARTESIAN_POINT ( 'NONE',  ( 201.5861714792528119, 52.66925088518574682, -5.382215963875594866 ) ) ;
#14230 = ORIENTED_EDGE ( 'NONE', *, *, #310, .F. ) ;
#14232 = EDGE_CURVE ( 'NONE', #831, #592, #13468, .T. ) ;
#14231 = PRODUCT_RELATED_PRODUCT_CATEGORY ( 'part', '', ( #10425 ) ) ;
#14233 = EDGE_CURVE ( 'NONE', #7696, #10895, #7419, .T. ) ;
#14234 = CARTESIAN_POINT ( 'NONE',  ( 190.0000000000000568, 16.03993994372673981, -7.458121719691109004E-14 ) ) ;
#14235 = FACE_BOUND ( 'NONE', #2610, .T. ) ;
#14236 = EDGE_CURVE ( 'NONE', #11227, #9977, #5003, .T. ) ;
#14237 = DIRECTION ( 'NONE',  ( 0.000000000000000000, 0.000000000000000000, 1.000000000000000000 ) ) ;
#14238 = AXIS2_PLACEMENT_3D ( 'NONE', #11719, #4440, #9273 ) ;
#14239 = ORIENTED_EDGE ( 'NONE', *, *, #4833, .F. ) ;
#14240 = CARTESIAN_POINT ( 'NONE',  ( 4.022812308926893010, 34.21572344292344070, 23.61251614551212441 ) ) ;
#14241 = CARTESIAN_POINT ( 'NONE',  ( 194.7891036845171300, 47.85977741052224133, -6.433373108600371815 ) ) ;
#14242 = ORIENTED_EDGE ( 'NONE', *, *, #9891, .T. ) ;
#14243 = CARTESIAN_POINT ( 'NONE',  ( -223.5918188539070002, 142.0538562971642307, 1.612306317632525854 ) ) ;
#14244 = CARTESIAN_POINT ( 'NONE',  ( -184.9748306402843809, 119.2867206268225999, 3.478895870929497036 ) ) ;
#14245 = CARTESIAN_POINT ( 'NONE',  ( -76.00000000000001421, 15.53993994372673804, 25.38206912977649310 ) ) ;
#14246 = DIRECTION ( 'NONE',  ( 0.000000000000000000, 0.000000000000000000, 1.000000000000000000 ) ) ;
#14247 = CARTESIAN_POINT ( 'NONE',  ( 205.4699394944333051, 33.88363592193200446, -7.930995773285529182 ) ) ;
#14248 = AXIS2_PLACEMENT_3D ( 'NONE', #12477, #14049, #10438 ) ;
#14249 = EDGE_CURVE ( 'NONE', #14286, #15409, #4746, .T. ) ;
#14250 = ORIENTED_EDGE ( 'NONE', *, *, #15246, .T. ) ;
#14251 = EDGE_CURVE ( 'NONE', #6589, #2137, #10892, .T. ) ;
#14252 = VERTEX_POINT ( 'NONE', #1386 ) ;
#14253 = DIRECTION ( 'NONE',  ( -0.000000000000000000, -0.000000000000000000, 1.000000000000000000 ) ) ;
#14254 = DIRECTION ( 'NONE',  ( 1.000000000000000000, 0.000000000000000000, 0.000000000000000000 ) ) ;
#14255 = AXIS2_PLACEMENT_3D ( 'NONE', #11166, #8796, #9988 ) ;
#14256 = DIRECTION ( 'NONE',  ( 0.000000000000000000, -0.000000000000000000, -1.000000000000000000 ) ) ;
#14257 = DIRECTION ( 'NONE',  ( -0.8731965799097685110, 0.4873681696970816324, 0.000000000000000000 ) ) ;
#14258 = CARTESIAN_POINT ( 'NONE',  ( -220.3095741282960773, 148.3879606264429754, -5.070227393135747107 ) ) ;
#14259 = ADVANCED_FACE ( 'NONE', ( #10015 ), #10540, .F. ) ;
#14260 = CYLINDRICAL_SURFACE ( 'NONE', #3364, 1.000000000000000888 ) ;
#14261 = AXIS2_PLACEMENT_3D ( 'NONE', #1798, #14968, #10408 ) ;
#14262 = CARTESIAN_POINT ( 'NONE',  ( 0.7145311798161593231, -4.618802153517259867, -7.999999999999979572 ) ) ;
#14263 = CYLINDRICAL_SURFACE ( 'NONE', #9706, 0.5000000000000004441 ) ;
#14264 = EDGE_CURVE ( 'NONE', #956, #4350, #8049, .T. ) ;
#14265 = DIRECTION ( 'NONE',  ( 0.000000000000000000, 0.000000000000000000, -1.000000000000000000 ) ) ;
#14266 = CARTESIAN_POINT ( 'NONE',  ( 64.00000000000005684, 62.13993994372673768, 13.30000000000070948 ) ) ;
#14267 = ORIENTED_EDGE ( 'NONE', *, *, #11440, .T. ) ;
#14268 = ORIENTED_EDGE ( 'NONE', *, *, #3965, .F. ) ;
#14269 = CARTESIAN_POINT ( 'NONE',  ( 70.26535645333922275, 38.79159067395544014, 10.00000000000000178 ) ) ;
#14270 = DIRECTION ( 'NONE',  ( -1.000000000000000000, 0.000000000000000000, 0.000000000000000000 ) ) ;
#14271 = SURFACE_STYLE_USAGE ( .BOTH. , #2438 ) ;
#14272 = FACE_OUTER_BOUND ( 'NONE', #6735, .T. ) ;
#14273 = AXIS2_PLACEMENT_3D ( 'NONE', #12069, #4893, #8606 ) ;
#14274 = AXIS2_PLACEMENT_3D ( 'NONE', #3847, #1454, #12356 ) ;
#14275 = ORIENTED_EDGE ( 'NONE', *, *, #12268, .F. ) ;
#14276 = ORIENTED_EDGE ( 'NONE', *, *, #10488, .F. ) ;
#14277 = CARTESIAN_POINT ( 'NONE',  ( 191.4384233894935505, 39.53989603517709384, -4.498996937958945175 ) ) ;
#14278 = ADVANCED_FACE ( 'NONE', ( #6224 ), #182, .T. ) ;
#14279 = CARTESIAN_POINT ( 'NONE',  ( 0.7145311798163155315, -4.618802153516981868, 8.000000000000007105 ) ) ;
#14280 = VERTEX_POINT ( 'NONE', #2826 ) ;
#14281 = CIRCLE ( 'NONE', #10520, 1.699999999999993072 ) ;
#14282 = DIRECTION ( 'NONE',  ( 0.000000000000000000, 0.000000000000000000, -1.000000000000000000 ) ) ;
#14283 = DIRECTION ( 'NONE',  ( -0.000000000000000000, 1.000000000000000000, -0.000000000000000000 ) ) ;
#14284 = DIRECTION ( 'NONE',  ( 0.000000000000000000, -0.000000000000000000, 1.000000000000000000 ) ) ;
#14285 = EDGE_LOOP ( 'NONE', ( #3694, #12904, #2078, #6588 ) ) ;
#14286 = VERTEX_POINT ( 'NONE', #3688 ) ;
#14287 = CARTESIAN_POINT ( 'NONE',  ( 122.5806775638430253, 45.00321902537314145, 10.00000000000000178 ) ) ;
#14288 = CARTESIAN_POINT ( 'NONE',  ( 183.0404880503516267, 40.86394065090267702, 5.000000000000000000 ) ) ;
#14289 = VERTEX_POINT ( 'NONE', #8519 ) ;
#14290 = CARTESIAN_POINT ( 'NONE',  ( -151.1267316678846839, 106.2776699442079433, 9.312033302791153488 ) ) ;
#14291 = CARTESIAN_POINT ( 'NONE',  ( 175.9483885134608272, -181.3058001507315566, 84.88378295107885663 ) ) ;
#14292 = CARTESIAN_POINT ( 'NONE',  ( 5.196152422706635576, -9.000000000000003553, 5.000000000000000000 ) ) ;
#14293 = VERTEX_POINT ( 'NONE', #14728 ) ;
#14294 = CARTESIAN_POINT ( 'NONE',  ( -111.2071507613730290, 58.10263819636593041, 10.00000000000000178 ) ) ;
#14295 = EDGE_CURVE ( 'NONE', #2689, #12599, #13307, .T. ) ;
#14296 = LINE ( 'NONE', #2229, #108 ) ;
#14297 = CARTESIAN_POINT ( 'NONE',  ( -206.8718859864436581, 149.4025266312245037, 2.500000000000000000 ) ) ;
#14298 = DIRECTION ( 'NONE',  ( 0.000000000000000000, -2.731481088613017720E-16, 1.000000000000000000 ) ) ;
#14299 = ORIENTED_EDGE ( 'NONE', *, *, #13085, .T. ) ;
#14300 = CARTESIAN_POINT ( 'NONE',  ( -194.3489852843322581, 137.1051365066642234, -4.640918829492427733 ) ) ;
#14301 = CARTESIAN_POINT ( 'NONE',  ( 191.4384233894935505, 39.53989603517709384, -4.498996937958945175 ) ) ;
#14302 = AXIS2_PLACEMENT_3D ( 'NONE', #11910, #10808, #7923 ) ;
#14303 = ORIENTED_EDGE ( 'NONE', *, *, #13694, .T. ) ;
#14304 = DIRECTION ( 'NONE',  ( 0.000000000000000000, 1.000000000000000000, 6.938893903907227145E-17 ) ) ;
#14305 = CARTESIAN_POINT ( 'NONE',  ( 0.4964154566687909442, 4.996589667937362478, 7.345652830558772273 ) ) ;
#14306 = EDGE_CURVE ( 'NONE', #12693, #4660, #3923, .T. ) ;
#14307 = CARTESIAN_POINT ( 'NONE',  ( -151.4086188282879277, 107.2728346664360259, 84.88378295107887084 ) ) ;
#14308 = AXIS2_PLACEMENT_3D ( 'NONE', #874, #11783, #13105 ) ;
#14309 = VERTEX_POINT ( 'NONE', #8675 ) ;
#14310 = CIRCLE ( 'NONE', #11805, 1.500000000000000666 ) ;
#14311 = VECTOR ( 'NONE', #9775, 1000.000000000000114 ) ;
#14312 = EDGE_CURVE ( 'NONE', #591, #2912, #14653, .T. ) ;
#14313 = LINE ( 'NONE', #7162, #15410 ) ;
#14314 = CARTESIAN_POINT ( 'NONE',  ( 202.3171501287270644, 32.63561614260228794, -6.547335233887139339 ) ) ;
#14315 = ORIENTED_EDGE ( 'NONE', *, *, #15205, .T. ) ;
#14316 = FACE_OUTER_BOUND ( 'NONE', #1182, .T. ) ;
#14317 = CARTESIAN_POINT ( 'NONE',  ( -199.4124801547868913, 127.6177204676982910, 3.478895870929493483 ) ) ;
#14318 = DIRECTION ( 'NONE',  ( -1.000000000000000000, 0.000000000000000000, 0.000000000000000000 ) ) ;
#14319 = FACE_OUTER_BOUND ( 'NONE', #12296, .T. ) ;
#14320 = DIRECTION ( 'NONE',  ( 0.000000000000000000, 1.000000000000000000, 8.673617379884035472E-17 ) ) ;
#14321 = AXIS2_PLACEMENT_3D ( 'NONE', #12874, #4351, #10361 ) ;
#14322 = VERTEX_POINT ( 'NONE', #6385 ) ;
#14323 = EDGE_LOOP ( 'NONE', ( #508, #9582, #13642, #13352 ) ) ;
#14324 = CARTESIAN_POINT ( 'NONE',  ( 190.0000000000000853, 15.53993994372673626, 52.49999999999997868 ) ) ;
#14325 = CARTESIAN_POINT ( 'NONE',  ( -132.4907271922243694, 117.2156449176087847, 0.000000000000000000 ) ) ;
#14326 = CARTESIAN_POINT ( 'NONE',  ( 207.0699012803337951, 46.20241706079673349, -2.754725152881798866 ) ) ;
#14327 = CIRCLE ( 'NONE', #7040, 0.5000000000000004441 ) ;
#14328 = LINE ( 'NONE', #2422, #5402 ) ;
#14329 = DIRECTION ( 'NONE',  ( -1.000000000000000000, 0.000000000000000000, 0.000000000000000000 ) ) ;
#14330 = CARTESIAN_POINT ( 'NONE',  ( -223.9140261897964876, 146.0620863009135348, -4.050555112215771913 ) ) ;
#14331 = CARTESIAN_POINT ( 'NONE',  ( -217.6520716543167282, 153.2380971607960589, 7.506281845139713305 ) ) ;
#14332 = EDGE_CURVE ( 'NONE', #13487, #14978, #953, .T. ) ;
#14333 = ADVANCED_FACE ( 'NONE', ( #8595, #13392 ), #12211, .F. ) ;
#14334 = EDGE_CURVE ( 'NONE', #5937, #9838, #2988, .T. ) ;
#14335 = DIRECTION ( 'NONE',  ( -0.000000000000000000, -0.000000000000000000, 1.000000000000000000 ) ) ;
#14336 = AXIS2_PLACEMENT_3D ( 'NONE', #5927, #9565, #7212 ) ;
#14337 = DIRECTION ( 'NONE',  ( -1.000000000000000000, -0.000000000000000000, 0.000000000000000000 ) ) ;
#14338 = DIRECTION ( 'NONE',  ( -0.000000000000000000, 1.000000000000000000, 6.938893903907227145E-17 ) ) ;
#14339 = AXIS2_PLACEMENT_3D ( 'NONE', #5640, #14226, #11877 ) ;
#14340 = LINE ( 'NONE', #5830, #13303 ) ;
#14341 = DIRECTION ( 'NONE',  ( -0.000000000000000000, -0.000000000000000000, -1.000000000000000000 ) ) ;
#14342 = ORIENTED_EDGE ( 'NONE', *, *, #14232, .F. ) ;
#14343 = ORIENTED_EDGE ( 'NONE', *, *, #8253, .T. ) ;
#14344 = FACE_OUTER_BOUND ( 'NONE', #9354, .T. ) ;
#14345 = DIRECTION ( 'NONE',  ( 1.000000000000000000, 0.000000000000000000, 0.000000000000000000 ) ) ;
#14346 =( GEOMETRIC_REPRESENTATION_CONTEXT ( 3 ) GLOBAL_UNCERTAINTY_ASSIGNED_CONTEXT ( ( #6913 ) ) GLOBAL_UNIT_ASSIGNED_CONTEXT ( ( #248, #12111, #14632 ) ) REPRESENTATION_CONTEXT ( 'NONE', 'WORKASPACE' ) );
#14347 = DIRECTION ( 'NONE',  ( 1.000000000000000000, 2.751328491981765035E-32, -3.965082230804130220E-16 ) ) ;
#14348 = SURFACE_SIDE_STYLE ('',( #9548 ) ) ;
#14349 = DIRECTION ( 'NONE',  ( 1.000000000000000000, 0.000000000000000000, -0.000000000000000000 ) ) ;
#14350 = DIRECTION ( 'NONE',  ( 0.000000000000000000, 0.000000000000000000, -1.000000000000000000 ) ) ;
#14351 = DIRECTION ( 'NONE',  ( 0.000000000000000000, 0.000000000000000000, 1.000000000000000000 ) ) ;
#14352 = ADVANCED_FACE ( 'NONE', ( #12593 ), #11505, .T. ) ;
#14353 = ORIENTED_EDGE ( 'NONE', *, *, #3168, .T. ) ;
#14354 = TOROIDAL_SURFACE ( 'NONE', #9836, 1.000000000000000000, 0.5000000000000000000 ) ;
#14355 = VECTOR ( 'NONE', #6106, 1000.000000000000000 ) ;
#14356 = ORIENTED_EDGE ( 'NONE', *, *, #3700, .T. ) ;
#14357 = AXIS2_PLACEMENT_3D ( 'NONE', #1168, #3031, #4274 ) ;
#14358 = CARTESIAN_POINT ( 'NONE',  ( 207.1167095084715868, 46.15093117762712893, -7.185265714380067337 ) ) ;
#14359 = CARTESIAN_POINT ( 'NONE',  ( -85.99999999999994316, 59.53993994372674337, 13.30000000000175575 ) ) ;
#14360 = VERTEX_POINT ( 'NONE', #1704 ) ;
#14362 = AXIS2_PLACEMENT_3D ( 'NONE', #1681, #1835, #7539 ) ;
#14361 = DIRECTION ( 'NONE',  ( 0.000000000000000000, -0.8660254037844380415, -0.5000000000000011102 ) ) ;
#14363 = CARTESIAN_POINT ( 'NONE',  ( -223.3687964238177983, 147.0389510131371367, 9.463477258803484560 ) ) ;
#14364 = ORIENTED_EDGE ( 'NONE', *, *, #2457, .T. ) ;
#14365 = ORIENTED_EDGE ( 'NONE', *, *, #2859, .T. ) ;
#14366 = CARTESIAN_POINT ( 'NONE',  ( 190.0000000000000568, -179.3058001507315566, -51.45141194869120937 ) ) ;
#14367 = LINE ( 'NONE', #11937, #7876 ) ;
#14368 = EDGE_LOOP ( 'NONE', ( #4203, #4183, #5964, #13983 ) ) ;
#14369 = CARTESIAN_POINT ( 'NONE',  ( -170.8906599468338641, 95.38134948400895041, 0.000000000000000000 ) ) ;
#14370 = EDGE_CURVE ( 'NONE', #13055, #14289, #6541, .T. ) ;
#14371 = CIRCLE ( 'NONE', #13108, 1.499999999999994449 ) ;
#14372 = EDGE_CURVE ( 'NONE', #3478, #12658, #10054, .T. ) ;
#14373 = DIRECTION ( 'NONE',  ( -0.000000000000000000, 1.000000000000000000, -0.000000000000000000 ) ) ;
#14374 = VERTEX_POINT ( 'NONE', #11342 ) ;
#14375 = ORIENTED_EDGE ( 'NONE', *, *, #11680, .T. ) ;
#14376 = AXIS2_PLACEMENT_3D ( 'NONE', #6881, #9322, #689 ) ;
#14377 = ORIENTED_EDGE ( 'NONE', *, *, #14690, .T. ) ;
#14378 = CARTESIAN_POINT ( 'NONE',  ( -222.0995690897442785, 149.3129710173510318, 2.431557144026069928 ) ) ;
#14379 = AXIS2_PLACEMENT_3D ( 'NONE', #6546, #9940, #14799 ) ;
#14380 = DIRECTION ( 'NONE',  ( 0.000000000000000000, -1.000000000000000000, -4.956352788505160310E-17 ) ) ;
#14381 = DIRECTION ( 'NONE',  ( 0.000000000000000000, 0.000000000000000000, 1.000000000000000000 ) ) ;
#14382 = ORIENTED_EDGE ( 'NONE', *, *, #9029, .F. ) ;
#14383 = ORIENTED_EDGE ( 'NONE', *, *, #7254, .T. ) ;
#14384 = CARTESIAN_POINT ( 'NONE',  ( -174.9627087613145306, 131.1742099673107305, -0.4568654681747568169 ) ) ;
#14385 = CARTESIAN_POINT ( 'NONE',  ( 204.2383844621755884, 51.59388984732451888, -2.501575441055724713 ) ) ;
#14386 = ORIENTED_EDGE ( 'NONE', *, *, #2719, .T. ) ;
#14387 = DIRECTION ( 'NONE',  ( -0.000000000000000000, 1.000000000000000000, -0.000000000000000000 ) ) ;
#14388 = DIRECTION ( 'NONE',  ( 0.000000000000000000, -0.1391731009600592484, -0.9902680687415712502 ) ) ;
#14389 = LINE ( 'NONE', #3660, #9831 ) ;
#14390 = AXIS2_PLACEMENT_3D ( 'NONE', #10212, #5475, #11629 ) ;
#14391 = PRESENTATION_LAYER_ASSIGNMENT (  '', '', ( #5592 ) ) ;
#14392 = ORIENTED_EDGE ( 'NONE', *, *, #5987, .F. ) ;
#14393 = ADVANCED_FACE ( 'NONE', ( #662 ), #12669, .F. ) ;
#14394 = PRODUCT_CONTEXT ( 'NONE', #5878, 'mechanical' ) ;
#14395 = CARTESIAN_POINT ( 'NONE',  ( 207.1288103955774318, 46.12660085639766550, -4.186765234109192768 ) ) ;
#14396 = VERTEX_POINT ( 'NONE', #1783 ) ;
#14397 = CARTESIAN_POINT ( 'NONE',  ( 200.1062858801516597, 40.86394065090267702, 5.000000000000000000 ) ) ;
#14398 = CYLINDRICAL_SURFACE ( 'NONE', #14491, 3.500000000000004885 ) ;
#14399 = CARTESIAN_POINT ( 'NONE',  ( -194.4337897068680547, 127.2572260587109554, 3.478895870929501033 ) ) ;
#14400 = CYLINDRICAL_SURFACE ( 'NONE', #4756, 3.500000000000003109 ) ;
#14401 = VERTEX_POINT ( 'NONE', #7728 ) ;
#14402 = CARTESIAN_POINT ( 'NONE',  ( -213.3956520262682091, 148.0073597223720583, 9.578254705571842109 ) ) ;
#14404 = CARTESIAN_POINT ( 'NONE',  ( 14.00000000000004086, 64.53993994372673626, 18.52500000000105018 ) ) ;
#14403 = VECTOR ( 'NONE', #1090, 1000.000000000000000 ) ;
#14405 = EDGE_LOOP ( 'NONE', ( #14382, #3502, #10481, #9005 ) ) ;
#14406 = ORIENTED_EDGE ( 'NONE', *, *, #13517, .T. ) ;
#14407 = AXIS2_PLACEMENT_3D ( 'NONE', #1101, #4580, #15531 ) ;
#14408 = LINE ( 'NONE', #15583, #9857 ) ;
#14409 = CARTESIAN_POINT ( 'NONE',  ( 190.5000000000000853, -178.8058001507315566, 52.19066787724494816 ) ) ;
#14410 = EDGE_CURVE ( 'NONE', #3554, #12934, #9792, .T. ) ;
#14411 = CARTESIAN_POINT ( 'NONE',  ( 178.0000000000000853, 16.03993994372673981, 7.553451883674125344E-16 ) ) ;
#14412 = DIRECTION ( 'NONE',  ( -1.000000000000000000, 0.000000000000000000, 0.000000000000000000 ) ) ;
#14413 = LINE ( 'NONE', #2660, #7337 ) ;
#14414 = CARTESIAN_POINT ( 'NONE',  ( -217.2422530631390600, 153.9507230298087848, 6.369419626229976927 ) ) ;
#14415 = LINE ( 'NONE', #9535, #837 ) ;
#14416 = CYLINDRICAL_SURFACE ( 'NONE', #8692, 3.500000000000003109 ) ;
#14417 = DIRECTION ( 'NONE',  ( 1.000000000000000000, -2.751328491981765035E-32, 3.965082230804130220E-16 ) ) ;
#14418 = DIRECTION ( 'NONE',  ( -1.000000000000000000, 0.000000000000000000, 0.000000000000000000 ) ) ;
#14419 = ORIENTED_EDGE ( 'NONE', *, *, #7899, .F. ) ;
#14420 =( NAMED_UNIT ( * ) SI_UNIT ( $, .STERADIAN. ) SOLID_ANGLE_UNIT ( ) );
#14421 = ORIENTED_EDGE ( 'NONE', *, *, #1670, .F. ) ;
#14422 = DIRECTION ( 'NONE',  ( -1.000000000000000000, 0.000000000000000000, 0.000000000000000000 ) ) ;
#14423 = DIRECTION ( 'NONE',  ( 1.000000000000000000, 0.000000000000000000, 0.000000000000000000 ) ) ;
#14424 = CARTESIAN_POINT ( 'NONE',  ( -70.00000000000000000, -181.3058001507315566, -42.95141194869119516 ) ) ;
#14425 = EDGE_CURVE ( 'NONE', #12461, #7800, #3485, .T. ) ;
#14426 = DIRECTION ( 'NONE',  ( 0.000000000000000000, 0.000000000000000000, 1.000000000000000000 ) ) ;
#14427 = DIRECTION ( 'NONE',  ( 0.000000000000000000, 0.000000000000000000, -1.000000000000000000 ) ) ;
#14429 = EDGE_CURVE ( 'NONE', #11107, #3604, #6270, .T. ) ;
#14428 = EDGE_CURVE ( 'NONE', #9410, #14199, #15066, .T. ) ;
#14430 = AXIS2_PLACEMENT_3D ( 'NONE', #10759, #11941, #13183 ) ;
#14431 = CYLINDRICAL_SURFACE ( 'NONE', #13343, 1.699999999999996625 ) ;
#14432 = CARTESIAN_POINT ( 'NONE',  ( -64.00000000000002842, 15.53993994372673981, -17.50000000000002487 ) ) ;
#14433 = ADVANCED_FACE ( 'NONE', ( #5342 ), #13942, .F. ) ;
#14434 = VERTEX_POINT ( 'NONE', #10164 ) ;
#14435 = ORIENTED_EDGE ( 'NONE', *, *, #4399, .F. ) ;
#14436 = CARTESIAN_POINT ( 'NONE',  ( 205.4911088677281725, 33.92184391926740972, -3.501858402168778639 ) ) ;
#14437 = LINE ( 'NONE', #1256, #273 ) ;
#14438 = ORIENTED_EDGE ( 'NONE', *, *, #8534, .F. ) ;
#14439 = CIRCLE ( 'NONE', #6407, 0.5000000000000004441 ) ;
#14440 = CARTESIAN_POINT ( 'NONE',  ( -223.2365180022060542, 142.7849184768047337, 6.010681374827787415 ) ) ;
#14441 = ORIENTED_EDGE ( 'NONE', *, *, #1489, .F. ) ;
#14442 = VERTEX_POINT ( 'NONE', #10086 ) ;
#14443 = CARTESIAN_POINT ( 'NONE',  ( 0.000000000000000000, 0.000000000000000000, 0.000000000000000000 ) ) ;
#14444 = DIRECTION ( 'NONE',  ( 1.000000000000000000, 0.000000000000000000, 0.000000000000000000 ) ) ;
#14445 = EDGE_LOOP ( 'NONE', ( #6492, #27 ) ) ;
#14446 = PLANE ( 'NONE',  #4645 ) ;
#14447 = DIRECTION ( 'NONE',  ( 1.000000000000000000, 0.000000000000000000, 0.000000000000000000 ) ) ;
#14448 = DIRECTION ( 'NONE',  ( 1.000000000000000000, 0.000000000000000000, 0.000000000000000000 ) ) ;
#14449 = AXIS2_PLACEMENT_3D ( 'NONE', #7643, #113, #2662 ) ;
#14450 = ORIENTED_EDGE ( 'NONE', *, *, #1796, .T. ) ;
#14451 = CIRCLE ( 'NONE', #4898, 1.000000000000000888 ) ;
#14452 = CYLINDRICAL_SURFACE ( 'NONE', #1112, 1.499999999999994449 ) ;
#14453 = CARTESIAN_POINT ( 'NONE',  ( 181.4384305232223369, 82.69763993231136112, 10.00000000000000178 ) ) ;
#14454 = EDGE_LOOP ( 'NONE', ( #3541, #2432, #14814, #2940 ) ) ;
#14455 = DIRECTION ( 'NONE',  ( 0.000000000000000000, 0.000000000000000000, -1.000000000000000000 ) ) ;
#14456 = ADVANCED_FACE ( 'NONE', ( #11269 ), #4074, .F. ) ;
#14457 = LINE ( 'NONE', #1123, #8094 ) ;
#14458 = LINE ( 'NONE', #9821, #10838 ) ;
#14459 = ORIENTED_EDGE ( 'NONE', *, *, #6543, .T. ) ;
#14460 = EDGE_LOOP ( 'NONE', ( #2832, #3162, #13708, #4847 ) ) ;
#14461 = CARTESIAN_POINT ( 'NONE',  ( -172.5271923976867470, 129.8359673051191123, -0.4588839673349612291 ) ) ;
#14462 = CARTESIAN_POINT ( 'NONE',  ( 202.9578473199472057, 32.84482942423175444, -9.656098271102047548 ) ) ;
#14463 = ORIENTED_EDGE ( 'NONE', *, *, #13041, .F. ) ;
#14464 = AXIS2_PLACEMENT_3D ( 'NONE', #7989, #9321, #15291 ) ;
#14465 = DIRECTION ( 'NONE',  ( -1.000000000000000000, 0.000000000000000000, 0.000000000000000000 ) ) ;
#14466 = CARTESIAN_POINT ( 'NONE',  ( -76.00000000000004263, 21.51947656765315386, 25.04661384777570987 ) ) ;
#14467 = DIRECTION ( 'NONE',  ( 0.000000000000000000, 0.000000000000000000, 1.000000000000000000 ) ) ;
#14468 = EDGE_LOOP ( 'NONE', ( #14588, #694, #9675, #6009 ) ) ;
#14469 = STYLED_ITEM ( 'NONE', ( #7449 ), #11106 ) ;
#14470 = EDGE_CURVE ( 'NONE', #12329, #7691, #6533, .T. ) ;
#14471 = CARTESIAN_POINT ( 'NONE',  ( 201.7905037730716913, 32.52922036567187547, -6.577523224799477930 ) ) ;
#14472 = VERTEX_POINT ( 'NONE', #1629 ) ;
#14473 = CARTESIAN_POINT ( 'NONE',  ( 0.000000000000000000, 6.928203230275514990, -4.000000000000003553 ) ) ;
#14474 = LINE ( 'NONE', #3438, #14985 ) ;
#14475 = CARTESIAN_POINT ( 'NONE',  ( -213.7840885461983760, 135.0504928752735339, -0.4555467707853347870 ) ) ;
#14476 = FACE_OUTER_BOUND ( 'NONE', #15365, .T. ) ;
#14477 = ORIENTED_EDGE ( 'NONE', *, *, #7764, .T. ) ;
#14478 = CARTESIAN_POINT ( 'NONE',  ( -177.2599095556795419, 121.3508012008377932, 9.485662293947264345 ) ) ;
#14479 = CARTESIAN_POINT ( 'NONE',  ( 184.0000000000000568, 17.53993994372673981, -13.99999999999999289 ) ) ;
#14480 = ORIENTED_EDGE ( 'NONE', *, *, #11926, .F. ) ;
#14481 = ORIENTED_EDGE ( 'NONE', *, *, #6856, .F. ) ;
#14482 = CARTESIAN_POINT ( 'NONE',  ( -63.50000000000002842, 15.53993994372673804, 24.94742576086838781 ) ) ;
#14483 = DIRECTION ( 'NONE',  ( 1.000000000000000000, 0.000000000000000000, 0.000000000000000000 ) ) ;
#14484 = VECTOR ( 'NONE', #11341, 1000.000000000000000 ) ;
#14485 = DIRECTION ( 'NONE',  ( -0.000000000000000000, 1.000000000000000000, -0.000000000000000000 ) ) ;
#14486 = FACE_OUTER_BOUND ( 'NONE', #3371, .T. ) ;
#14487 = CARTESIAN_POINT ( 'NONE',  ( 190.0000000000000853, 14.97035339324670744, 37.58005016923963382 ) ) ;
#14488 = CARTESIAN_POINT ( 'NONE',  ( -216.9323607303195729, 154.4852837081892574, 5.108206056088243407 ) ) ;
#14489 = DIRECTION ( 'NONE',  ( 0.000000000000000000, 0.000000000000000000, 1.000000000000000000 ) ) ;
#14490 = CARTESIAN_POINT ( 'NONE',  ( -64.00000000000002842, 15.53993994372673981, 25.38206912977650376 ) ) ;
#14491 = AXIS2_PLACEMENT_3D ( 'NONE', #8202, #15571, #11970 ) ;
#14492 = ADVANCED_FACE ( 'NONE', ( #6622 ), #14071, .F. ) ;
#14493 = CARTESIAN_POINT ( 'NONE',  ( -85.27455057502459113, 65.19100426474074084, 10.00000000000000178 ) ) ;
#14494 = DIRECTION ( 'NONE',  ( -0.000000000000000000, 1.000000000000000000, 1.156482317317871725E-16 ) ) ;
#14495 = DIRECTION ( 'NONE',  ( 0.000000000000000000, 0.000000000000000000, -1.000000000000000000 ) ) ;
#14496 = ORIENTED_EDGE ( 'NONE', *, *, #5152, .T. ) ;
#14497 =( NAMED_UNIT ( * ) PLANE_ANGLE_UNIT ( ) SI_UNIT ( $, .RADIAN. ) );
#14498 = ORIENTED_EDGE ( 'NONE', *, *, #11111, .T. ) ;
#14499 = CARTESIAN_POINT ( 'NONE',  ( -76.50000000000001421, -178.6666270497714777, -18.18093594598673945 ) ) ;
#14500 = DIRECTION ( 'NONE',  ( -1.000000000000000000, 0.000000000000000000, 0.000000000000000000 ) ) ;
#14501 = DIRECTION ( 'NONE',  ( 0.000000000000000000, -0.000000000000000000, 1.000000000000000000 ) ) ;
#14502 = CYLINDRICAL_SURFACE ( 'NONE', #11425, 1.499999999999999778 ) ;
#14503 = CARTESIAN_POINT ( 'NONE',  ( -110.0000000000000426, 19.53993994372674337, 24.99999999999999645 ) ) ;
#14504 = CARTESIAN_POINT ( 'NONE',  ( 64.00000000000005684, 64.53993994372673626, 11.50000000000069811 ) ) ;
#14505 = CARTESIAN_POINT ( 'NONE',  ( -206.8762397066792005, 149.3947262580036863, 3.478855109513426580 ) ) ;
#14506 = CIRCLE ( 'NONE', #8233, 3.499999999999999556 ) ;
#14507 =( REPRESENTATION_RELATIONSHIP ('NONE','NONE', #3298, #11876 ) REPRESENTATION_RELATIONSHIP_WITH_TRANSFORMATION ( #12863 )SHAPE_REPRESENTATION_RELATIONSHIP( ) );
#14508 = VECTOR ( 'NONE', #2970, 1000.000000000000114 ) ;
#14510 = ORIENTED_EDGE ( 'NONE', *, *, #2967, .T. ) ;
#14509 = EDGE_CURVE ( 'NONE', #7288, #8073, #3735, .T. ) ;
#14511 = ORIENTED_EDGE ( 'NONE', *, *, #10888, .F. ) ;
#14512 = CARTESIAN_POINT ( 'NONE',  ( 205.4526553411199359, 47.86694802938139759, -2.633259993550844502 ) ) ;
#14513 = PRODUCT_DEFINITION ( 'UNKNOWN', '', #13309, #1566 ) ;
#14514 = CARTESIAN_POINT ( 'NONE',  ( -224.5769159865018594, 144.8744151739456925, 3.251642181181148672 ) ) ;
#14515 = ORIENTED_EDGE ( 'NONE', *, *, #1886, .T. ) ;
#14516 = CARTESIAN_POINT ( 'NONE',  ( -221.1308609718745117, 146.8914367518880226, 9.717582667742421521 ) ) ;
#14517 = ORIENTED_EDGE ( 'NONE', *, *, #7183, .T. ) ;
#14518 = EDGE_CURVE ( 'NONE', #6255, #12471, #7293, .T. ) ;
#14519 = DIRECTION ( 'NONE',  ( 0.000000000000000000, -0.5000000000000012212, 0.8660254037844380415 ) ) ;
#14520 = CARTESIAN_POINT ( 'NONE',  ( 211.8897246948783106, 42.46053108337658699, -4.442978748809460754 ) ) ;
#14521 = CIRCLE ( 'NONE', #2695, 3.500000000000004885 ) ;
#14522 = EDGE_LOOP ( 'NONE', ( #12990, #7910, #12621, #8063 ) ) ;
#14523 = CARTESIAN_POINT ( 'NONE',  ( -76.50000000000001421, -179.3058001507315566, -30.31842631998718574 ) ) ;
#14524 = DIRECTION ( 'NONE',  ( 0.000000000000000000, 0.1391731009600592484, 0.9902680687415712502 ) ) ;
#14525 = DIRECTION ( 'NONE',  ( 0.000000000000000000, -1.000000000000000000, 0.000000000000000000 ) ) ;
#14526 = VECTOR ( 'NONE', #7658, 1000.000000000000000 ) ;
#14527 = EDGE_LOOP ( 'NONE', ( #4566, #9746, #4411, #945 ) ) ;
#14528 = ADVANCED_FACE ( 'NONE', ( #4385 ), #9216, .F. ) ;
#14529 = EDGE_CURVE ( 'NONE', #15193, #2866, #11309, .T. ) ;
#14530 = PLANE ( 'NONE',  #13546 ) ;
#14531 = EDGE_LOOP ( 'NONE', ( #8317, #11489, #13839, #5725 ) ) ;
#14532 = DIRECTION ( 'NONE',  ( -0.000000000000000000, 1.000000000000000000, -0.000000000000000000 ) ) ;
#14533 = CARTESIAN_POINT ( 'NONE',  ( -151.5642236857922001, 108.2694729682366841, -4.924812526309171545 ) ) ;
#14534 = ORIENTED_EDGE ( 'NONE', *, *, #8380, .F. ) ;
#14535 = ORIENTED_EDGE ( 'NONE', *, *, #4994, .T. ) ;
#14536 = CARTESIAN_POINT ( 'NONE',  ( -193.1449676018668526, 139.3614456044060148, -2.963320117457103109 ) ) ;
#14537 = CARTESIAN_POINT ( 'NONE',  ( 198.9111841706756536, 32.15857605477618364, -5.308824953579920347 ) ) ;
#14538 = ORIENTED_EDGE ( 'NONE', *, *, #1181, .F. ) ;
#14539 = CARTESIAN_POINT ( 'NONE',  ( -61.94838851346079167, -178.8058001507315566, -30.31842631998718574 ) ) ;
#14540 = FACE_OUTER_BOUND ( 'NONE', #6499, .T. ) ;
#14541 = DIRECTION ( 'NONE',  ( -0.000000000000000000, 1.000000000000000000, -0.000000000000000000 ) ) ;
#14542 = EDGE_CURVE ( 'NONE', #3604, #8586, #10476, .T. ) ;
#14543 = VERTEX_POINT ( 'NONE', #8123 ) ;
#14544 = CARTESIAN_POINT ( 'NONE',  ( 201.5722569949026877, 29.04292258031605556, -3.626438834624695406 ) ) ;
#14545 = EDGE_LOOP ( 'NONE', ( #10543, #12388, #5288, #7749, #13267, #11848, #1120, #10402, #7593, #13804, #15454, #5391, #15376, #11102, #1353, #7510, #11660 ) ) ;
#14546 = DIRECTION ( 'NONE',  ( -0.000000000000000000, -0.000000000000000000, 1.000000000000000000 ) ) ;
#14547 = CARTESIAN_POINT ( 'NONE',  ( -132.4907271922243694, 117.2156449176087847, 5.000000000000000000 ) ) ;
#14548 = AXIS2_PLACEMENT_3D ( 'NONE', #9468, #4639, #15596 ) ;
#14549 = CARTESIAN_POINT ( 'NONE',  ( -200.1353104204616500, 130.1171604195963880, -2.964974570226841522 ) ) ;
#14550 = CARTESIAN_POINT ( 'NONE',  ( -70.00000000000000000, 15.53993994372673626, 47.49999999999997868 ) ) ;
#14551 = CARTESIAN_POINT ( 'NONE',  ( -220.8021227237918254, 143.2564083082033619, 7.918248976830615682 ) ) ;
#14552 = CARTESIAN_POINT ( 'NONE',  ( 122.5806775638430253, 45.00321902537314145, 10.00000000000000178 ) ) ;
#14553 = ORIENTED_EDGE ( 'NONE', *, *, #8173, .F. ) ;
#14554 = VERTEX_POINT ( 'NONE', #4622 ) ;
#14555 = LINE ( 'NONE', #10713, #9346 ) ;
#14556 = CARTESIAN_POINT ( 'NONE',  ( -76.00000000000007105, -178.8058001507315566, 65.31842631998698323 ) ) ;
#14557 = AXIS2_PLACEMENT_3D ( 'NONE', #12288, #1712, #193 ) ;
#14558 = DIRECTION ( 'NONE',  ( 0.000000000000000000, 1.000000000000000000, 0.000000000000000000 ) ) ;
#14559 = DIRECTION ( 'NONE',  ( -3.965082230804130220E-16, 1.090924371466202084E-47, 1.000000000000000000 ) ) ;
#14560 = EDGE_CURVE ( 'NONE', #9742, #5551, #2175, .T. ) ;
#14561 = CARTESIAN_POINT ( 'NONE',  ( -223.3090784427782864, 142.6032858358233000, -0.6846340373356000208 ) ) ;
#14562 = AXIS2_PLACEMENT_3D ( 'NONE', #10650, #7648, #7341 ) ;
#14563 = B_SPLINE_CURVE_WITH_KNOTS ( 'NONE', 3,
 ( #3935, #12222, #11131, #127 ),
 .UNSPECIFIED., .F., .F.,
 ( 4, 4 ),
 ( 2.380742993382810214E-07, 0.001606744326298690335 ),
 .UNSPECIFIED. ) ;
#14564 = DIRECTION ( 'NONE',  ( 0.000000000000000000, 0.000000000000000000, 1.000000000000000000 ) ) ;
#14565 = DIRECTION ( 'NONE',  ( 0.000000000000000000, 0.000000000000000000, 1.000000000000000000 ) ) ;
#14566 = VECTOR ( 'NONE', #3173, 1000.000000000000000 ) ;
#14567 = CARTESIAN_POINT ( 'NONE',  ( -185.2055264765504887, 137.3096093875189467, 2.500000000000000000 ) ) ;
#14568 = CIRCLE ( 'NONE', #2227, 0.5000000000000004441 ) ;
#14569 = DIRECTION ( 'NONE',  ( -0.000000000000000000, 1.000000000000000000, -0.000000000000000000 ) ) ;
#14570 = DIRECTION ( 'NONE',  ( 0.000000000000000000, 0.000000000000000000, -1.000000000000000000 ) ) ;
#14571 = ORIENTED_EDGE ( 'NONE', *, *, #4767, .F. ) ;
#14572 = DIRECTION ( 'NONE',  ( 0.000000000000000000, 0.000000000000000000, 1.000000000000000000 ) ) ;
#14573 = AXIS2_PLACEMENT_3D ( 'NONE', #10302, #13764, #11251 ) ;
#14574 = EDGE_CURVE ( 'NONE', #14943, #10460, #15263, .T. ) ;
#14575 = ORIENTED_EDGE ( 'NONE', *, *, #11033, .F. ) ;
#14576 = CARTESIAN_POINT ( 'NONE',  ( 5.196152422706635576, -9.000000000000003553, 0.000000000000000000 ) ) ;
#14577 = DIRECTION ( 'NONE',  ( 0.8731965799097685110, -0.4873681696970816879, -0.000000000000000000 ) ) ;
#14578 = DIRECTION ( 'NONE',  ( 0.8731965799097682890, -0.4873681696970819099, 0.000000000000000000 ) ) ;
#14579 = CARTESIAN_POINT ( 'NONE',  ( -64.00000000000002842, 16.03993994372673981, 7.553451883674125344E-16 ) ) ;
#14580 = PLANE ( 'NONE',  #5213 ) ;
#14581 = DIRECTION ( 'NONE',  ( 0.000000000000000000, -1.000000000000000000, 0.000000000000000000 ) ) ;
#14582 = CARTESIAN_POINT ( 'NONE',  ( 64.00000000000005684, 56.53993994372675047, 15.00000000000070166 ) ) ;
#14583 = VECTOR ( 'NONE', #1711, 1000.000000000000000 ) ;
#14584 = AXIS2_PLACEMENT_3D ( 'NONE', #10897, #3543, #7348 ) ;
#14585 = VERTEX_POINT ( 'NONE', #6852 ) ;
#14586 = CIRCLE ( 'NONE', #12326, 0.5000000000000004441 ) ;
#14587 = EDGE_CURVE ( 'NONE', #6998, #7301, #2224, .T. ) ;
#14588 = ORIENTED_EDGE ( 'NONE', *, *, #8034, .F. ) ;
#14589 = CARTESIAN_POINT ( 'NONE',  ( 191.3780708436489704, 41.94285887643944477, -4.625461852610818880 ) ) ;
#14590 = CARTESIAN_POINT ( 'NONE',  ( -220.6606568355639411, 151.8910081918378125, 7.146912864506841601 ) ) ;
#14591 = ORIENTED_EDGE ( 'NONE', *, *, #6450, .T. ) ;
#14592 = VECTOR ( 'NONE', #11653, 1000.000000000000000 ) ;
#14594 = B_SPLINE_CURVE_WITH_KNOTS ( 'NONE', 3,
 ( #4788, #1379, #13385, #12130, #9854, #7410, #11981, #3846 ),
 .UNSPECIFIED., .F., .F.,
 ( 4, 2, 2, 4 ),
 ( 0.01336725832182607265, 0.01453745201803763321, 0.01570764571424919376, 0.01804803310667231833 ),
 .UNSPECIFIED. ) ;
#14593 = CARTESIAN_POINT ( 'NONE',  ( -223.4360080598686693, 146.9185308168432584, 7.053220276998304783 ) ) ;
#14595 = ORIENTED_EDGE ( 'NONE', *, *, #5457, .F. ) ;
#14596 = LINE ( 'NONE', #3796, #11829 ) ;
#14597 = CARTESIAN_POINT ( 'NONE',  ( 190.6325473606148648, 48.03985028950570779, -6.316729457008944948 ) ) ;
#14598 = AXIS2_PLACEMENT_3D ( 'NONE', #9488, #3244, #11538 ) ;
#14599 = ORIENTED_EDGE ( 'NONE', *, *, #8760, .F. ) ;
#14600 = CYLINDRICAL_SURFACE ( 'NONE', #10202, 1.700000000000007061 ) ;
#14601 = CARTESIAN_POINT ( 'NONE',  ( -110.0000000000000426, 19.53993994372674337, 24.99999999999999645 ) ) ;
#14602 = ADVANCED_FACE ( 'NONE', ( #11972, #12910, #5890 ), #5734, .F. ) ;
#14603 = VECTOR ( 'NONE', #12911, 1000.000000000000114 ) ;
#14604 = CARTESIAN_POINT ( 'NONE',  ( 190.5000000000000568, -178.6666270497714777, -18.18093594598673945 ) ) ;
#14605 = ORIENTED_EDGE ( 'NONE', *, *, #4894, .F. ) ;
#14606 = CIRCLE ( 'NONE', #7562, 0.5000000000000004441 ) ;
#14607 = AXIS2_PLACEMENT_3D ( 'NONE', #15161, #9193, #3255 ) ;
#14608 = VECTOR ( 'NONE', #9989, 1000.000000000000000 ) ;
#14609 = EDGE_LOOP ( 'NONE', ( #6201, #13782, #15401, #5000 ) ) ;
#14610 = PLANE ( 'NONE',  #11712 ) ;
#14611 = DIRECTION ( 'NONE',  ( -0.8950274278067241740, 0.4460111024107797362, -0.000000000000000000 ) ) ;
#14612 = EDGE_LOOP ( 'NONE', ( #2966, #5941 ) ) ;
#14613 = CARTESIAN_POINT ( 'NONE',  ( 190.2479883433758800, 63.36949047362622167, 0.000000000000000000 ) ) ;
#14614 = DIRECTION ( 'NONE',  ( 1.000000000000000000, 0.000000000000000000, 0.000000000000000000 ) ) ;
#14615 = AXIS2_PLACEMENT_3D ( 'NONE', #5706, #5629, #14060 ) ;
#14616 = VERTEX_POINT ( 'NONE', #2337 ) ;
#14617 = ORIENTED_EDGE ( 'NONE', *, *, #11908, .F. ) ;
#14618 = CARTESIAN_POINT ( 'NONE',  ( -209.2730951545231335, 145.1348166524657302, -4.640918829492436615 ) ) ;
#14619 = CARTESIAN_POINT ( 'NONE',  ( 203.0658429208174880, 48.83360436048501896, -0.9158339742359169477 ) ) ;
#14620 = AXIS2_PLACEMENT_3D ( 'NONE', #794, #2875, #10137 ) ;
#14621 = ORIENTED_EDGE ( 'NONE', *, *, #12884, .F. ) ;
#14622 = CIRCLE ( 'NONE', #1007, 4.499999999999950262 ) ;
#14623 = CARTESIAN_POINT ( 'NONE',  ( -157.6477983077465694, 110.1970436846185066, 0.000000000000000000 ) ) ;
#14624 = LINE ( 'NONE', #241, #8980 ) ;
#14625 = EDGE_CURVE ( 'NONE', #13113, #14692, #10825, .T. ) ;
#14627 = ADVANCED_FACE ( 'NONE', ( #2014 ), #1142, .F. ) ;
#14626 = EDGE_CURVE ( 'NONE', #3946, #10635, #7004, .T. ) ;
#14628 = DIRECTION ( 'NONE',  ( 1.000000000000000000, -0.000000000000000000, -0.000000000000000000 ) ) ;
#14629 = CONICAL_SURFACE ( 'NONE', #14880, 3.525000000000000355, 0.7853981633973787790 ) ;
#14630 = ORIENTED_EDGE ( 'NONE', *, *, #12610, .F. ) ;
#14631 = AXIS2_PLACEMENT_3D ( 'NONE', #8990, #8827, #3857 ) ;
#14632 =( NAMED_UNIT ( * ) SI_UNIT ( $, .STERADIAN. ) SOLID_ANGLE_UNIT ( ) );
#14633 = CARTESIAN_POINT ( 'NONE',  ( 198.8102040144913758, 32.17279782253822162, -0.7412068558913099681 ) ) ;
#14634 = ORIENTED_EDGE ( 'NONE', *, *, #10517, .T. ) ;
#14635 = PLANE ( 'NONE',  #4576 ) ;
#14636 = CARTESIAN_POINT ( 'NONE',  ( -217.0245320789650805, 154.3266673407848941, -0.6962477592939494420 ) ) ;
#14637 = CARTESIAN_POINT ( 'NONE',  ( -185.2102393155530535, 125.0770951282925409, -4.642206099734998759 ) ) ;
#14638 = CYLINDRICAL_SURFACE ( 'NONE', #8802, 0.4999999999999996114 ) ;
#14639 = VERTEX_POINT ( 'NONE', #11814 ) ;
#14640 = CARTESIAN_POINT ( 'NONE',  ( -208.4006302466032992, 134.8330880460140122, 7.918248976830637886 ) ) ;
#14641 = CARTESIAN_POINT ( 'NONE',  ( 208.8119045081773777, 39.60750423734790360, -5.989029428842635561 ) ) ;
#14642 = ORIENTED_EDGE ( 'NONE', *, *, #2285, .F. ) ;
#14643 = ORIENTED_EDGE ( 'NONE', *, *, #3662, .F. ) ;
#14644 = CIRCLE ( 'NONE', #14138, 0.5000000000000004441 ) ;
#14645 = DIRECTION ( 'NONE',  ( -1.000000000000000000, 0.000000000000000000, 0.000000000000000000 ) ) ;
#14646 = CARTESIAN_POINT ( 'NONE',  ( -150.4086188282879277, 107.2728346664360259, -4.856732557889654522 ) ) ;
#14647 = CLOSED_SHELL ( 'NONE', ( #1899, #8192, #535, #4500, #4474, #13320, #7625, #12275, #1523, #7701, #13752, #1648, #11631, #12152, #3525, #12529, #1059, #8656, #6694, #1694, #3917, #8816, #6320, #13261, #13391, #15613, #3240, #11136, #8567, #12032, #7193, #12811, #12982, #1201 ) ) ;
#14648 = CARTESIAN_POINT ( 'NONE',  ( -223.2622533207028539, 142.6949529005080421, -0.9050894319243404373 ) ) ;
#14649 = CARTESIAN_POINT ( 'NONE',  ( 119.0556775638430196, 45.00321902537314145, 10.00000000000000178 ) ) ;
#14650 = AXIS2_PLACEMENT_3D ( 'NONE', #5860, #9566, #2299 ) ;
#14651 = DIRECTION ( 'NONE',  ( -0.000000000000000000, -0.000000000000000000, -1.000000000000000000 ) ) ;
#14652 = CARTESIAN_POINT ( 'NONE',  ( -193.1820620331849341, 139.2949851078578831, 7.919662025281897222 ) ) ;
#14653 = LINE ( 'NONE', #4960, #14311 ) ;
#14654 = AXIS2_PLACEMENT_3D ( 'NONE', #97, #8576, #6206 ) ;
#14655 = DIRECTION ( 'NONE',  ( 0.000000000000000000, 0.000000000000000000, 1.000000000000000000 ) ) ;
#14656 = ORIENTED_EDGE ( 'NONE', *, *, #346, .T. ) ;
#14657 = DIRECTION ( 'NONE',  ( 0.000000000000000000, -1.000000000000000000, -1.156482317317871478E-16 ) ) ;
#14658 = EDGE_CURVE ( 'NONE', #927, #15023, #1735, .T. ) ;
#14659 = EDGE_LOOP ( 'NONE', ( #5894, #14118 ) ) ;
#14660 = DIRECTION ( 'NONE',  ( 0.000000000000000000, 0.000000000000000000, 1.000000000000000000 ) ) ;
#14661 = CARTESIAN_POINT ( 'NONE',  ( -224.2927258533811425, 145.3835864077571216, 2.431557144026069928 ) ) ;
#14662 = DIRECTION ( 'NONE',  ( 0.000000000000000000, 1.000000000000000000, 0.000000000000000000 ) ) ;
#14663 = DIRECTION ( 'NONE',  ( 1.000000000000000000, 0.000000000000000000, 0.000000000000000000 ) ) ;
#14664 = CIRCLE ( 'NONE', #8139, 0.5000000000000004441 ) ;
#14665 = DIRECTION ( 'NONE',  ( 1.000000000000000000, 0.000000000000000000, 0.000000000000000000 ) ) ;
#14666 = CARTESIAN_POINT ( 'NONE',  ( -177.5673841713239085, 132.5493133318365437, 5.434754235172600367 ) ) ;
#14667 = CIRCLE ( 'NONE', #1551, 0.4000000000000001887 ) ;
#14668 = VERTEX_POINT ( 'NONE', #10787 ) ;
#14669 = CARTESIAN_POINT ( 'NONE',  ( 194.7691866843436799, 33.87697957786221536, -2.559886773443665220 ) ) ;
#14670 = CARTESIAN_POINT ( 'NONE',  ( -219.5914105103326790, 153.8067308268499858, 4.439047251926309556 ) ) ;
#14671 = ORIENTED_EDGE ( 'NONE', *, *, #2694, .T. ) ;
#14672 = CARTESIAN_POINT ( 'NONE',  ( -221.5674180155096167, 146.0573998878414841, 9.414961245066379547 ) ) ;
#14673 = ORIENTED_EDGE ( 'NONE', *, *, #967, .F. ) ;
#14674 = CARTESIAN_POINT ( 'NONE',  ( -173.6511438682215953, 117.1093890634716672, -2.227947778868676565 ) ) ;
#14676 = CLOSED_SHELL ( 'NONE', ( #11266, #7266, #135, #7983, #3508, #10009, #1878, #4109, #513, #6072 ) ) ;
#14675 = CIRCLE ( 'NONE', #561, 0.5000000000000004441 ) ;
#14677 = CARTESIAN_POINT ( 'NONE',  ( 203.8654192366412587, 29.97399779996683833, -8.095401878506494953 ) ) ;
#14678 = EDGE_LOOP ( 'NONE', ( #4149, #10750 ) ) ;
#14679 = CARTESIAN_POINT ( 'NONE',  ( 2.000000000000000000, 1.587713240271468207, -2.750000000000000000 ) ) ;
#14680 = CARTESIAN_POINT ( 'NONE',  ( 0.000000000000000000, 6.928203230275514990, -4.000000000000003553 ) ) ;
#14681 = EDGE_CURVE ( 'NONE', #13871, #6214, #10546, .T. ) ;
#14682 = LINE ( 'NONE', #14986, #3097 ) ;
#14683 = ORIENTED_EDGE ( 'NONE', *, *, #15575, .F. ) ;
#14684 = VERTEX_POINT ( 'NONE', #7169 ) ;
#14685 = SURFACE_STYLE_USAGE ( .BOTH. , #14762 ) ;
#14686 = DIRECTION ( 'NONE',  ( 1.000000000000000000, 0.000000000000000000, 0.000000000000000000 ) ) ;
#14687 = ORIENTED_EDGE ( 'NONE', *, *, #3081, .T. ) ;
#14688 = CIRCLE ( 'NONE', #578, 0.5000000000000004441 ) ;
#14689 = DIRECTION ( 'NONE',  ( -0.3663757939738424008, 0.9304669674900000187, 0.000000000000000000 ) ) ;
#14690 = EDGE_CURVE ( 'NONE', #7288, #3704, #2253, .T. ) ;
#14691 = CARTESIAN_POINT ( 'NONE',  ( -152.2217123724471435, 107.8691177927835838, -4.760088435541713459 ) ) ;
#14692 = VERTEX_POINT ( 'NONE', #3366 ) ;
#14693 = EDGE_LOOP ( 'NONE', ( #13379, #10263 ) ) ;
#14694 = DIRECTION ( 'NONE',  ( 0.000000000000000000, 4.956352788505162775E-17, -1.000000000000000000 ) ) ;
#14695 = CARTESIAN_POINT ( 'NONE',  ( 198.8634854004546071, 49.55149448133588663, -6.680369717582868461 ) ) ;
#14696 = EDGE_LOOP ( 'NONE', ( #4101, #5291, #2317, #2567 ) ) ;
#14697 = CIRCLE ( 'NONE', #6904, 3.752352628381527833 ) ;
#14698 = DIRECTION ( 'NONE',  ( 0.000000000000000000, 0.000000000000000000, 1.000000000000000000 ) ) ;
#14699 = CARTESIAN_POINT ( 'NONE',  ( 0.2456200930617507272, -1.587713240271640958, -2.750000000000000888 ) ) ;
#14700 = CYLINDRICAL_SURFACE ( 'NONE', #7836, 0.5000000000000004441 ) ;
#14701 = EDGE_CURVE ( 'NONE', #4918, #8392, #15422, .T. ) ;
#14702 = FACE_OUTER_BOUND ( 'NONE', #6339, .T. ) ;
#14703 = CARTESIAN_POINT ( 'NONE',  ( 188.3636875860777593, 42.62859381388609137, -4.500015676459212521 ) ) ;
#14704 = ORIENTED_EDGE ( 'NONE', *, *, #2388, .T. ) ;
#14705 = CARTESIAN_POINT ( 'NONE',  ( -70.00000000000000000, -201.3058001507315566, 77.95141194869098911 ) ) ;
#14706 = CYLINDRICAL_SURFACE ( 'NONE', #9717, 0.4999999999999996114 ) ;
#14707 = AXIS2_PLACEMENT_3D ( 'NONE', #8742, #1382, #6220 ) ;
#14708 = CARTESIAN_POINT ( 'NONE',  ( -216.0630845075784805, 143.0974466248333954, -4.642206099735013858 ) ) ;
#14710 = ADVANCED_FACE ( 'NONE', ( #4780 ), #14400, .F. ) ;
#14709 = FACE_OUTER_BOUND ( 'NONE', #3672, .T. ) ;
#14711 = EDGE_CURVE ( 'NONE', #3245, #3263, #2498, .T. ) ;
#14712 = VERTEX_POINT ( 'NONE', #12984 ) ;
#14713 = CARTESIAN_POINT ( 'NONE',  ( -200.1466204956978459, 130.0968966444285968, 7.918248976830634334 ) ) ;
#14714 = CARTESIAN_POINT ( 'NONE',  ( 198.8863654052626657, 49.55881746625484396, -3.681704842056328086 ) ) ;
#14715 = AXIS2_PLACEMENT_3D ( 'NONE', #8738, #13531, #12355 ) ;
#14716 = EDGE_LOOP ( 'NONE', ( #7230, #5737, #7224, #7843, #14961 ) ) ;
#14717 = ORIENTED_EDGE ( 'NONE', *, *, #2642, .F. ) ;
#14718 = EDGE_CURVE ( 'NONE', #14008, #830, #980, .T. ) ;
#14719 = PLANE ( 'NONE',  #11958 ) ;
#14720 = CARTESIAN_POINT ( 'NONE',  ( 6.399999999999999467, -9.237604307034018802, 2.775557561562891351E-14 ) ) ;
#14721 = FACE_OUTER_BOUND ( 'NONE', #6796, .T. ) ;
#14722 = AXIS2_PLACEMENT_3D ( 'NONE', #9701, #15515, #11988 ) ;
#14723 = FACE_OUTER_BOUND ( 'NONE', #6750, .T. ) ;
#14724 = DIRECTION ( 'NONE',  ( 0.000000000000000000, 1.000000000000000000, 0.000000000000000000 ) ) ;
#14725 = ADVANCED_FACE ( 'NONE', ( #2726 ), #11101, .F. ) ;
#14726 = EDGE_CURVE ( 'NONE', #10971, #8310, #5522, .T. ) ;
#14727 = CARTESIAN_POINT ( 'NONE',  ( -214.8759442515754188, 153.8597017879883424, 3.478855109513426580 ) ) ;
#14728 = CARTESIAN_POINT ( 'NONE',  ( -136.9508382163321585, 108.2653706395415583, 5.000000000000000000 ) ) ;
#14729 = DIRECTION ( 'NONE',  ( 0.000000000000000000, 0.000000000000000000, -1.000000000000000000 ) ) ;
#14730 = EDGE_LOOP ( 'NONE', ( #10768, #22, #12332, #2258 ) ) ;
#14731 = CARTESIAN_POINT ( 'NONE',  ( -88.79955057502458260, 65.19100426474074084, 10.00000000000000178 ) ) ;
#14732 = ORIENTED_EDGE ( 'NONE', *, *, #137, .T. ) ;
#14733 = ORIENTED_EDGE ( 'NONE', *, *, #1006, .T. ) ;
#14734 = CARTESIAN_POINT ( 'NONE',  ( -151.2970693524540877, 108.2755082659018768, 9.813568765712858522 ) ) ;
#14735 = FACE_OUTER_BOUND ( 'NONE', #3226, .T. ) ;
#14736 = CARTESIAN_POINT ( 'NONE',  ( 5.799999999999999822, 0.000000000000000000, 0.000000000000000000 ) ) ;
#14737 =( NAMED_UNIT ( * ) PLANE_ANGLE_UNIT ( ) SI_UNIT ( $, .RADIAN. ) );
#14738 = FACE_OUTER_BOUND ( 'NONE', #13635, .T. ) ;
#14739 = DIRECTION ( 'NONE',  ( -3.862829527358613429E-15, 0.9902680687415705840, -0.1391731009600641333 ) ) ;
#14740 = FACE_OUTER_BOUND ( 'NONE', #2710, .T. ) ;
#14741 = CARTESIAN_POINT ( 'NONE',  ( -174.7889847475609599, 131.4854638080208247, 3.478855109783925315 ) ) ;
#14742 = ORIENTED_EDGE ( 'NONE', *, *, #4402, .F. ) ;
#14743 = ADVANCED_FACE ( 'NONE', ( #6368 ), #7550, .F. ) ;
#14744 = CARTESIAN_POINT ( 'NONE',  ( 198.8872864542346974, 32.16591232847088122, -2.310211674251309688 ) ) ;
#14745 = CARTESIAN_POINT ( 'NONE',  ( -223.1382750711026404, 147.4519662024128479, 7.419826817990093026 ) ) ;
#14746 = VERTEX_POINT ( 'NONE', #9760 ) ;
#14747 = CARTESIAN_POINT ( 'NONE',  ( -219.5899114050779417, 153.8094167092946520, 7.921877796732283095 ) ) ;
#14748 = ORIENTED_EDGE ( 'NONE', *, *, #2039, .T. ) ;
#14749 = CARTESIAN_POINT ( 'NONE',  ( -169.8738088132719213, 123.8770777559960692, -4.653609069845229484 ) ) ;
#14750 = CARTESIAN_POINT ( 'NONE',  ( 13.07968152355895874, 460.3807876674321165, 0.000000000000000000 ) ) ;
#14751 = CIRCLE ( 'NONE', #14248, 3.500000000000003109 ) ;
#14752 = VERTEX_POINT ( 'NONE', #12348 ) ;
#14753 = CARTESIAN_POINT ( 'NONE',  ( -85.99999999999994316, 64.53993994372673626, 11.47500000000174758 ) ) ;
#14754 = DIRECTION ( 'NONE',  ( 0.000000000000000000, -1.000000000000000000, 0.000000000000000000 ) ) ;
#14755 = TOROIDAL_SURFACE ( 'NONE', #893, 1.000000000000000000, 0.5000000000000000000 ) ;
#14756 = EDGE_CURVE ( 'NONE', #5773, #9626, #15586, .T. ) ;
#14757 = DIRECTION ( 'NONE',  ( 0.000000000000000000, -0.9902680687415702510, 0.1391731009600660485 ) ) ;
#14758 = VERTEX_POINT ( 'NONE', #7401 ) ;
#14759 = ADVANCED_FACE ( 'NONE', ( #12191 ), #12074, .T. ) ;
#14760 = DIRECTION ( 'NONE',  ( 0.000000000000000000, -1.000000000000000000, -1.156482317317871725E-16 ) ) ;
#14761 = ORIENTED_EDGE ( 'NONE', *, *, #11252, .T. ) ;
#14762 = SURFACE_SIDE_STYLE ('',( #9735 ) ) ;
#14763 = CARTESIAN_POINT ( 'NONE',  ( -156.5362488319127579, 111.1997172840843575, 9.813568765712854969 ) ) ;
#14764 = ORIENTED_EDGE ( 'NONE', *, *, #244, .T. ) ;
#14765 = VECTOR ( 'NONE', #5556, 1000.000000000000000 ) ;
#14766 = DIRECTION ( 'NONE',  ( 0.000000000000000000, 4.956352788505162775E-17, -1.000000000000000000 ) ) ;
#14767 = DIRECTION ( 'NONE',  ( -0.8731965799097685110, 0.4873681696970816324, 0.000000000000000000 ) ) ;
#14768 = ORIENTED_EDGE ( 'NONE', *, *, #3073, .F. ) ;
#14769 = EDGE_LOOP ( 'NONE', ( #15599, #6364, #13470, #3247 ) ) ;
#14770 = CARTESIAN_POINT ( 'NONE',  ( -63.50000000000002842, 19.53993994372674692, -17.50000000000002487 ) ) ;
#14771 = CARTESIAN_POINT ( 'NONE',  ( 194.8381067511959372, 47.88228248201940573, -3.436395123936771601 ) ) ;
#14772 = ORIENTED_EDGE ( 'NONE', *, *, #2996, .T. ) ;
#14773 = DIRECTION ( 'NONE',  ( -1.000000000000000000, 0.000000000000000000, 0.000000000000000000 ) ) ;
#14774 = DIRECTION ( 'NONE',  ( -0.000000000000000000, 1.000000000000000000, -0.000000000000000000 ) ) ;
#14775 = AXIS2_PLACEMENT_3D ( 'NONE', #9785, #8303, #4725 ) ;
#14776 = CARTESIAN_POINT ( 'NONE',  ( -108.0000000000000568, 64.53993994372673626, 10.00000000000000178 ) ) ;
#14777 = DIRECTION ( 'NONE',  ( 0.000000000000000000, -1.156482317317871725E-16, 1.000000000000000000 ) ) ;
#14778 = ORIENTED_EDGE ( 'NONE', *, *, #1850, .F. ) ;
#14779 = CARTESIAN_POINT ( 'NONE',  ( -64.00000000000002842, 15.03993994372673981, -3.075184203610571654 ) ) ;
#14780 = CARTESIAN_POINT ( 'NONE',  ( -219.8172205651076752, 149.3079862779945302, -4.999365138195623892 ) ) ;
#14781 = CARTESIAN_POINT ( 'NONE',  ( -193.5420962672365022, 128.8371742780315969, -2.964974570226833084 ) ) ;
#14782 = ORIENTED_EDGE ( 'NONE', *, *, #5603, .F. ) ;
#14783 = CARTESIAN_POINT ( 'NONE',  ( -209.2398179475638926, 133.3202902034983595, 5.434137442415948094 ) ) ;
#14784 = CIRCLE ( 'NONE', #13790, 1.700000000000000178 ) ;
#14785 = CARTESIAN_POINT ( 'NONE',  ( 205.4319281802536068, 33.87189768065903905, -1.932853472788024440 ) ) ;
#14786 = VERTEX_POINT ( 'NONE', #7322 ) ;
#14787 = ORIENTED_EDGE ( 'NONE', *, *, #4302, .T. ) ;
#14788 = EDGE_CURVE ( 'NONE', #620, #12158, #14327, .T. ) ;
#14789 = CARTESIAN_POINT ( 'NONE',  ( 164.0000000000000568, 59.53993994372674337, 16.70000000000000995 ) ) ;
#14790 = FACE_OUTER_BOUND ( 'NONE', #13246, .T. ) ;
#14791 = LINE ( 'NONE', #12581, #5805 ) ;
#14792 = EDGE_CURVE ( 'NONE', #14996, #2654, #26, .T. ) ;
#14793 = DIRECTION ( 'NONE',  ( -0.000000000000000000, 1.000000000000000000, 1.156482317317871725E-16 ) ) ;
#14794 = CARTESIAN_POINT ( 'NONE',  ( 164.0000000000000568, 64.53993994372673626, 15.00000000000000355 ) ) ;
#14795 = APPLICATION_CONTEXT ( 'automotive_design' ) ;
#14796 = CARTESIAN_POINT ( 'NONE',  ( -179.9311234670130943, 134.3555102485248369, 3.478855109513426580 ) ) ;
#14797 = DIRECTION ( 'NONE',  ( 0.000000000000000000, 0.000000000000000000, 1.000000000000000000 ) ) ;
#14798 = ORIENTED_EDGE ( 'NONE', *, *, #4796, .F. ) ;
#14799 = DIRECTION ( 'NONE',  ( -1.000000000000000000, 0.000000000000000000, -0.000000000000000000 ) ) ;
#14800 = VECTOR ( 'NONE', #10483, 1000.000000000000000 ) ;
#14801 = ORIENTED_EDGE ( 'NONE', *, *, #13841, .T. ) ;
#14802 = ORIENTED_EDGE ( 'NONE', *, *, #10492, .F. ) ;
#14803 = CARTESIAN_POINT ( 'NONE',  ( 178.0000000000000853, 14.97035339324670922, -2.580050169239785696 ) ) ;
#14804 = FACE_OUTER_BOUND ( 'NONE', #10276, .T. ) ;
#14805 = VECTOR ( 'NONE', #15070, 1000.000000000000000 ) ;
#14806 = CARTESIAN_POINT ( 'NONE',  ( 5.799999999999999822, -6.928203230275514990, 4.000000000000058620 ) ) ;
#14807 = LINE ( 'NONE', #2916, #13960 ) ;
#14808 = CARTESIAN_POINT ( 'NONE',  ( -63.50000000000002842, -178.8058001507315566, 65.31842631998698323 ) ) ;
#14809 = DIRECTION ( 'NONE',  ( 0.000000000000000000, 1.000000000000000000, 6.938893903907227145E-17 ) ) ;
#14810 = CARTESIAN_POINT ( 'NONE',  ( -198.7725242955204692, 144.3921638819772113, 5.434754235172606585 ) ) ;
#14811 = EDGE_CURVE ( 'NONE', #8410, #14322, #8059, .T. ) ;
#14812 = ADVANCED_FACE ( 'NONE', ( #14476 ), #13451, .F. ) ;
#14813 = EDGE_CURVE ( 'NONE', #5911, #11697, #5764, .T. ) ;
#14814 = ORIENTED_EDGE ( 'NONE', *, *, #734, .T. ) ;
#14815 = VECTOR ( 'NONE', #5425, 1000.000000000000000 ) ;
#14816 = CARTESIAN_POINT ( 'NONE',  ( 190.5000000000000568, 15.03993994372673981, -2.075184203610571210 ) ) ;
#14817 = CARTESIAN_POINT ( 'NONE',  ( -222.6528199517674125, 148.3217352523010959, 7.791448390692321979 ) ) ;
#14818 = ORIENTED_EDGE ( 'NONE', *, *, #8871, .T. ) ;
#14819 = CARTESIAN_POINT ( 'NONE',  ( -221.4570519113204341, 150.4641414006810294, 7.827120672804973367 ) ) ;
#14820 = ORIENTED_EDGE ( 'NONE', *, *, #4078, .F. ) ;
#14821 = CARTESIAN_POINT ( 'NONE',  ( 190.5000000000000853, 17.53993994372673626, 52.49999999999997868 ) ) ;
#14822 = DIRECTION ( 'NONE',  ( 0.000000000000000000, 0.000000000000000000, -1.000000000000000000 ) ) ;
#14823 = ADVANCED_FACE ( 'NONE', ( #7471 ), #14638, .T. ) ;
#14824 = ORIENTED_EDGE ( 'NONE', *, *, #7859, .T. ) ;
#14825 = AXIS2_PLACEMENT_3D ( 'NONE', #7133, #1032, #10988 ) ;
#14826 = LINE ( 'NONE', #7838, #5378 ) ;
#14827 = CARTESIAN_POINT ( 'NONE',  ( 190.5000000000000853, 15.53993994372673626, 52.49999999999997868 ) ) ;
#14828 = AXIS2_PLACEMENT_3D ( 'NONE', #9034, #14350, #3547 ) ;
#14829 = CIRCLE ( 'NONE', #9806, 0.5000000000000004441 ) ;
#14830 = LINE ( 'NONE', #4027, #8164 ) ;
#14831 = ORIENTED_EDGE ( 'NONE', *, *, #4052, .T. ) ;
#14832 = SHAPE_DEFINITION_REPRESENTATION ( #4623, #3387 ) ;
#14833 = EDGE_LOOP ( 'NONE', ( #1862, #14161, #14515, #7730 ) ) ;
#14834 = DIRECTION ( 'NONE',  ( -0.000000000000000000, 1.000000000000000000, 6.938893903907222067E-15 ) ) ;
#14835 = AXIS2_PLACEMENT_3D ( 'NONE', #13198, #3587, #160 ) ;
#14836 = CARTESIAN_POINT ( 'NONE',  ( -157.6477983077465979, 110.3242255389737068, 9.455162786586084778 ) ) ;
#14837 = VERTEX_POINT ( 'NONE', #8434 ) ;
#14838 = PLANE ( 'NONE',  #3169 ) ;
#14839 = TOROIDAL_SURFACE ( 'NONE', #718, 1.000000000000000000, 0.5000000000000000000 ) ;
#14840 = ADVANCED_FACE ( 'NONE', ( #14709 ), #8655, .F. ) ;
#14841 = EDGE_CURVE ( 'NONE', #9826, #1584, #3996, .T. ) ;
#14842 = CARTESIAN_POINT ( 'NONE',  ( -85.27455057502459113, 65.19100426474074084, 0.000000000000000000 ) ) ;
#14843 = EDGE_LOOP ( 'NONE', ( #5960, #14496, #279, #7883 ) ) ;
#14844 = EDGE_LOOP ( 'NONE', ( #3004, #10473 ) ) ;
#14845 = DIRECTION ( 'NONE',  ( 0.000000000000000000, 1.734723475976806306E-15, -1.000000000000000000 ) ) ;
#14846 = CARTESIAN_POINT ( 'NONE',  ( 193.1249951165660548, 46.22013307728793308, -3.310989833511668756 ) ) ;
#14847 = EDGE_CURVE ( 'NONE', #5951, #11227, #12266, .T. ) ;
#14848 = ORIENTED_EDGE ( 'NONE', *, *, #13957, .F. ) ;
#14849 = CARTESIAN_POINT ( 'NONE',  ( 1.960598928577951748E-15, -6.732211846623379792, 4.339467034331228490 ) ) ;
#14850 = CARTESIAN_POINT ( 'NONE',  ( 126.1056775638430310, 45.00321902537314145, 10.00000000000000178 ) ) ;
#14851 = AXIS2_PLACEMENT_3D ( 'NONE', #12960, #2309, #2 ) ;
#14852 = CARTESIAN_POINT ( 'NONE',  ( -156.8931177578041343, 109.2182220046010173, -4.336802791931503087 ) ) ;
#14853 = CARTESIAN_POINT ( 'NONE',  ( -63.50000000000002842, -178.7362136002515172, 52.68580191161573367 ) ) ;
#14854 = AXIS2_PLACEMENT_3D ( 'NONE', #9873, #12070, #12294 ) ;
#14855 = CYLINDRICAL_SURFACE ( 'NONE', #2002, 3.500000000000003109 ) ;
#14856 = VECTOR ( 'NONE', #9418, 1000.000000000000000 ) ;
#14857 = AXIS2_PLACEMENT_3D ( 'NONE', #11395, #7620, #1598 ) ;
#14858 = ORIENTED_EDGE ( 'NONE', *, *, #6377, .T. ) ;
#14859 = DIRECTION ( 'NONE',  ( -1.669238443041287922E-16, 1.000000000000000000, 0.000000000000000000 ) ) ;
#14860 = DIRECTION ( 'NONE',  ( 0.000000000000000000, -0.1391731009600592484, -0.9902680687415712502 ) ) ;
#14861 = CARTESIAN_POINT ( 'NONE',  ( -219.6417540138374704, 145.3326194796887023, -4.642206099735023628 ) ) ;
#14862 = LINE ( 'NONE', #13683, #1466 ) ;
#14863 = ORIENTED_EDGE ( 'NONE', *, *, #534, .F. ) ;
#14864 = CARTESIAN_POINT ( 'NONE',  ( -190.6501653245252044, 127.3085702864440520, 7.918248976830637886 ) ) ;
#14865 = CARTESIAN_POINT ( 'NONE',  ( 193.0454511798755846, 35.63895119138042133, -1.116400838283317043 ) ) ;
#14866 = ORIENTED_EDGE ( 'NONE', *, *, #11033, .T. ) ;
#14867 = CARTESIAN_POINT ( 'NONE',  ( 190.5000000000000568, 15.53993994372673981, -17.50000000000002487 ) ) ;
#14868 = CARTESIAN_POINT ( 'NONE',  ( -216.7216729069047005, 154.8463875879168086, 3.280095325655492111 ) ) ;
#14869 = AXIS2_PLACEMENT_3D ( 'NONE', #2126, #933, #5760 ) ;
#14870 = EDGE_CURVE ( 'NONE', #5551, #11247, #5264, .T. ) ;
#14871 = CARTESIAN_POINT ( 'NONE',  ( -76.50000000000004263, 15.53993994372673626, 52.49999999999997868 ) ) ;
#14872 = VECTOR ( 'NONE', #13396, 1000.000000000000000 ) ;
#14873 = AXIS2_PLACEMENT_3D ( 'NONE', #6066, #4791, #7181 ) ;
#14874 = CARTESIAN_POINT ( 'NONE',  ( -76.00000000000004263, -179.8058001507315566, 65.31842631998698323 ) ) ;
#14875 = ADVANCED_FACE ( 'NONE', ( #13524 ), #6027, .T. ) ;
#14876 = VERTEX_POINT ( 'NONE', #10149 ) ;
#14877 = LINE ( 'NONE', #13617, #3397 ) ;
#14878 = CARTESIAN_POINT ( 'NONE',  ( -174.9866660642990155, 131.1312866983521701, 5.432615396193912538 ) ) ;
#14879 = CARTESIAN_POINT ( 'NONE',  ( -64.00000000000002842, -179.8058001507315566, 65.31842631998698323 ) ) ;
#14880 = AXIS2_PLACEMENT_3D ( 'NONE', #11222, #14911, #11376 ) ;
#14881 = FACE_OUTER_BOUND ( 'NONE', #10589, .T. ) ;
#14882 = ORIENTED_EDGE ( 'NONE', *, *, #12225, .T. ) ;
#14884 = DIRECTION ( 'NONE',  ( -1.000000000000000000, 0.000000000000000000, 0.000000000000000000 ) ) ;
#14883 = VECTOR ( 'NONE', #15538, 1000.000000000000000 ) ;
#14885 = EDGE_CURVE ( 'NONE', #810, #7406, #15079, .T. ) ;
#14886 = EDGE_LOOP ( 'NONE', ( #10811, #12931, #13927, #8230 ) ) ;
#14887 = ORIENTED_EDGE ( 'NONE', *, *, #14066, .T. ) ;
#14888 = DIRECTION ( 'NONE',  ( -1.000000000000000000, 0.000000000000000000, 0.000000000000000000 ) ) ;
#14889 = CARTESIAN_POINT ( 'NONE',  ( -85.27455057502459113, 65.19100426474074084, 7.600000000000002309 ) ) ;
#14890 =( LENGTH_UNIT ( ) NAMED_UNIT ( * ) SI_UNIT ( .MILLI., .METRE. ) );
#14891 = DIRECTION ( 'NONE',  ( 0.000000000000000000, 0.000000000000000000, -1.000000000000000000 ) ) ;
#14892 = CARTESIAN_POINT ( 'NONE',  ( 178.0000000000000853, -178.9449732516916072, 64.32815825124539799 ) ) ;
#14893 = CARTESIAN_POINT ( 'NONE',  ( -220.1893657699912694, 152.7354001160292682, -1.484330510404517911 ) ) ;
#14894 = VERTEX_POINT ( 'NONE', #1768 ) ;
#14895 = AXIS2_PLACEMENT_3D ( 'NONE', #771, #6723, #11608 ) ;
#14896 = CARTESIAN_POINT ( 'NONE',  ( 190.5000000000000568, -179.3058001507315566, 52.19066787724494816 ) ) ;
#14897 = VECTOR ( 'NONE', #6889, 1000.000000000000000 ) ;
#14898 = CARTESIAN_POINT ( 'NONE',  ( 0.000000000000000000, 0.000000000000000000, 0.000000000000000000 ) ) ;
#14899 = CARTESIAN_POINT ( 'NONE',  ( 202.9147226314038051, 48.88641379461363101, -0.9068510277452211943 ) ) ;
#14900 = DIRECTION ( 'NONE',  ( -0.000000000000000000, 1.000000000000000000, 1.156482317317871725E-16 ) ) ;
#14901 = EDGE_LOOP ( 'NONE', ( #772, #5176, #3021, #7107 ) ) ;
#14902 = CARTESIAN_POINT ( 'NONE',  ( -221.2092521592557546, 150.9081135545043821, 7.674399710142353115 ) ) ;
#14904 = ADVANCED_FACE ( 'NONE', ( #8971 ), #4510, .T. ) ;
#14903 = EDGE_CURVE ( 'NONE', #2217, #11305, #14862, .T. ) ;
#14905 = ORIENTED_EDGE ( 'NONE', *, *, #822, .F. ) ;
#14906 = CARTESIAN_POINT ( 'NONE',  ( -168.1636048451761951, 126.9411766215776396, -1.100011624693940870 ) ) ;
#14907 = DIRECTION ( 'NONE',  ( -0.000000000000000000, 1.000000000000000000, -0.000000000000000000 ) ) ;
#14908 = VECTOR ( 'NONE', #13938, 1000.000000000000114 ) ;
#14909 = ORIENTED_EDGE ( 'NONE', *, *, #445, .T. ) ;
#14910 = LINE ( 'NONE', #13805, #14217 ) ;
#14911 = DIRECTION ( 'NONE',  ( -0.000000000000000000, -0.000000000000000000, 1.000000000000000000 ) ) ;
#14912 = EDGE_CURVE ( 'NONE', #6496, #8328, #14829, .T. ) ;
#14913 = CIRCLE ( 'NONE', #789, 0.5000000000000004441 ) ;
#14914 = CARTESIAN_POINT ( 'NONE',  ( 2.000000000000000000, 1.587713240271470427, 2.750000000000000888 ) ) ;
#14915 = ORIENTED_EDGE ( 'NONE', *, *, #13956, .F. ) ;
#14916 = APPLICATION_PROTOCOL_DEFINITION ( 'draft international standard', 'automotive_design', 1998, #5939 ) ;
#14917 = AXIS2_PLACEMENT_3D ( 'NONE', #5164, #14777, #10942 ) ;
#14918 = EDGE_LOOP ( 'NONE', ( #7431, #13900, #7327, #7008 ) ) ;
#14919 = DIRECTION ( 'NONE',  ( -0.000000000000000000, -0.000000000000000000, 1.000000000000000000 ) ) ;
#14920 = ORIENTED_EDGE ( 'NONE', *, *, #13262, .F. ) ;
#14921 = CARTESIAN_POINT ( 'NONE',  ( 190.0000000000000853, 15.53993994372673804, 37.49999999999991473 ) ) ;
#14922 = EDGE_CURVE ( 'NONE', #13965, #12005, #8556, .T. ) ;
#14923 = DIRECTION ( 'NONE',  ( -0.7900120431063439863, 0.6130913241491352528, 0.000000000000000000 ) ) ;
#14924 = VERTEX_POINT ( 'NONE', #7712 ) ;
#14925 = ORIENTED_EDGE ( 'NONE', *, *, #1508, .F. ) ;
#14926 = CARTESIAN_POINT ( 'NONE',  ( 177.5000000000000853, -179.8058001507315566, -17.76585208085566947 ) ) ;
#14927 = CARTESIAN_POINT ( 'NONE',  ( 114.0000000000000568, 62.13993994372673768, 15.00000000000035172 ) ) ;
#14928 = ORIENTED_EDGE ( 'NONE', *, *, #10755, .T. ) ;
#14929 = CARTESIAN_POINT ( 'NONE',  ( -70.00000000000000000, 17.53993994372673981, -10.99999999999999822 ) ) ;
#14930 = CARTESIAN_POINT ( 'NONE',  ( -64.00000000000002842, -179.3058001507315566, 52.19066787724494816 ) ) ;
#14931 = FACE_OUTER_BOUND ( 'NONE', #2527, .T. ) ;
#14932 = AXIS2_PLACEMENT_3D ( 'NONE', #14914, #3881, #4106 ) ;
#14933 = DIRECTION ( 'NONE',  ( -1.000000000000000000, 0.000000000000000000, 0.000000000000000000 ) ) ;
#14934 = B_SPLINE_SURFACE_WITH_KNOTS ( 'NONE', 3, 3, ( 
 ( #4624, #103, #6058, #14247, #2341, #8278, #983, #5892, #3446, #4944, #30, #8584, #13376, #8437, #13216, #13053, #12043, #2256, #1216, #15502, #11975, #1145, #5972, #4135, #1449, #8661, #14714, #5175, #12194, #9923, #2730, #6372, #8733, #11183, #10002, #14785, #7474, #5328, #13608, #12501, #10072, #8897, #5022, #258 ),
 ( #5099, #10153, #2813, #3910, #13527, #14641, #2892, #12270, #11255, #7553, #334, #6286, #12426, #11105, #1618, #3978, #8810, #6528, #7635, #12352, #6449, #13686, #2965, #7715, #11328, #1374, #1535, #410, #14945, #5247, #8974, #14865, #1692, #4061, #489, #13767, #6212, #3839, #11025, #174, #9849, #13454, #2653, #14076 ),
 ( #12810, #4526, #5491, #3270, #9046, #9129, #15097, #5570, #7949, #11563, #4446, #5643, #887, #12574, #809, #11491, #4289, #1844, #8111, #1771, #15327, #6914, #4369, #10305, #575, #5412, #1999, #10462, #13929, #12894, #6757, #4209, #3118, #7791, #6837, #2080, #12733, #651, #6688, #1921, #15250, #11647, #13846, #9279 ),
 ( #3045, #7874, #14155, #11724, #5719, #10381, #15174, #9356, #6606, #727, #10530, #9205, #11410, #10228, #15022, #12657, #14002, #3192, #8023, #11880, #6114, #7232, #1128, #15485, #4928, #14229, #2397, #4849, #13274, #10933, #4762, #9585, #5950, #3350, #3501, #13121, #12026, #1195, #4680, #3583, #7070, #14385, #9745, #11797 ),
 ( #10771, #6034, #14462, #11956, #1052, #10856, #3427, #8336, #8187, #12970, #88, #2157, #7150, #4607, #9430, #2321, #10694, #5876, #6992, #11, #8260, #8418, #13194, #9508, #3656, #1282, #965, #13035, #2236, #5793, #14301, #10617, #15557, #9667, #8492, #2470, #7304, #12102, #15407, #11163, #8876, #2873, #8791, #13668 ),
 ( #7694, #12483, #8717, #6354, #12411, #9985, #8561, #317, #12331, #6195, #14695, #8639, #6509, #3819, #11007, #1433, #7534, #14537, #12253, #5080, #13509, #11084, #2712, #1517, #5157, #9825, #1675, #14771, #14846, #1595, #11237, #7386, #2635, #393, #3963, #7457, #11308, #13588, #6269, #237, #1356, #5231, #14619, #2793 ) ),
 .UNSPECIFIED., .T., .F., .F.,
 ( 4, 2, 4 ),
 ( 4, 2, 2, 2, 2, 2, 2, 2, 2, 2, 2, 2, 2, 2, 2, 2, 2, 2, 2, 2, 2, 4 ),
 ( 0.000000000000000000, 0.5000000000000000000, 1.000000000000000000 ),
 ( 0.000000000000000000, 0.01154246058414762008, 0.06319472280952896648, 0.1156547325041140800, 0.1678637871092111822, 0.2189476930995808979, 0.2714221776790743945, 0.3227197530690046334, 0.3747274728241424824, 0.4267432521036158555, 0.4780248536244998681, 0.5305055628088307662, 0.5815973485975094448, 0.6337991395759137170, 0.6855599279679012170, 0.7371634071600560167, 0.7894711232639126663, 0.8405207634104210346, 0.8929453349049019106, 0.9452650328228678900, 0.9965476795071586125, 1.000000000000000000 ),
 .UNSPECIFIED. ) ;
#14935 = AXIS2_PLACEMENT_3D ( 'NONE', #3800, #8622, #8476 ) ;
#14936 = EDGE_CURVE ( 'NONE', #8234, #10763, #8807, .T. ) ;
#14937 = CARTESIAN_POINT ( 'NONE',  ( 6.399999999999999467, 0.000000000000000000, 0.000000000000000000 ) ) ;
#14938 = ORIENTED_EDGE ( 'NONE', *, *, #8462, .T. ) ;
#14939 = SURFACE_STYLE_USAGE ( .BOTH. , #13521 ) ;
#14940 = LINE ( 'NONE', #15091, #9465 ) ;
#14941 = CARTESIAN_POINT ( 'NONE',  ( -193.1449676018668526, 139.3614456044060148, -2.963320117457103109 ) ) ;
#14942 = DIRECTION ( 'NONE',  ( -0.000000000000000000, 1.000000000000000000, -0.000000000000000000 ) ) ;
#14943 = VERTEX_POINT ( 'NONE', #1688 ) ;
#14944 = CARTESIAN_POINT ( 'NONE',  ( -201.1640730962011219, 128.1953734590158263, 1.515400478619091773 ) ) ;
#14945 = CARTESIAN_POINT ( 'NONE',  ( 193.1683668805158334, 46.28448754599228465, -1.741988976065122152 ) ) ;
#14946 = VECTOR ( 'NONE', #4161, 1000.000000000000227 ) ;
#14947 = ORIENTED_EDGE ( 'NONE', *, *, #10504, .F. ) ;
#14948 = DIRECTION ( 'NONE',  ( -1.000000000000000000, 0.000000000000000000, 0.000000000000000000 ) ) ;
#14949 = DIRECTION ( 'NONE',  ( -1.000000000000000000, -0.000000000000000000, -0.000000000000000000 ) ) ;
#14950 = DIRECTION ( 'NONE',  ( 1.000000000000000000, 0.000000000000000000, 0.000000000000000000 ) ) ;
#14951 = VECTOR ( 'NONE', #12688, 1000.000000000000000 ) ;
#14952 = DIRECTION ( 'NONE',  ( -1.000000000000000000, 0.000000000000000000, 0.000000000000000000 ) ) ;
#14953 = ORIENTED_EDGE ( 'NONE', *, *, #2246, .F. ) ;
#14954 = CYLINDRICAL_SURFACE ( 'NONE', #11223, 0.5000000000000004441 ) ;
#14955 = CARTESIAN_POINT ( 'NONE',  ( -207.9892458934089632, 147.4169567187306029, 7.919662025281897222 ) ) ;
#14956 = DIRECTION ( 'NONE',  ( 0.000000000000000000, 0.000000000000000000, -1.000000000000000000 ) ) ;
#14957 = CARTESIAN_POINT ( 'NONE',  ( -157.6477983077465410, 110.3243625741235974, -4.592095542101950478 ) ) ;
#14958 = ORIENTED_EDGE ( 'NONE', *, *, #6901, .T. ) ;
#14959 = CARTESIAN_POINT ( 'NONE',  ( 178.0000000000000853, 15.53993994372674159, -17.50000000000002487 ) ) ;
#14960 = ORIENTED_EDGE ( 'NONE', *, *, #13086, .T. ) ;
#14961 = ORIENTED_EDGE ( 'NONE', *, *, #12915, .F. ) ;
#14962 = CARTESIAN_POINT ( 'NONE',  ( 119.0556775638430196, 45.00321902537314145, 10.00000000000000178 ) ) ;
#14963 = CARTESIAN_POINT ( 'NONE',  ( 0.000000000000000000, -2.381569860407202643, 1.375000000000004663 ) ) ;
#14964 = AXIS2_PLACEMENT_3D ( 'NONE', #10925, #2547, #4993 ) ;
#14965 = CARTESIAN_POINT ( 'NONE',  ( 114.0000000000000568, 56.53993994372675047, 15.00000000000035172 ) ) ;
#14966 = CARTESIAN_POINT ( 'NONE',  ( -219.2661329852160748, 154.3895165730399412, -2.326617110117079612 ) ) ;
#14967 = AXIS2_PLACEMENT_3D ( 'NONE', #1657, #11454, #616 ) ;
#14968 = DIRECTION ( 'NONE',  ( -1.000000000000000000, -0.000000000000000000, -0.000000000000000000 ) ) ;
#14969 = EDGE_LOOP ( 'NONE', ( #11050, #12771, #9684, #1576 ) ) ;
#14970 = EDGE_CURVE ( 'NONE', #6505, #3793, #3115, .T. ) ;
#14971 = CARTESIAN_POINT ( 'NONE',  ( -76.50000000000004263, 15.03993994372673804, 38.07518420361041933 ) ) ;
#14972 = CARTESIAN_POINT ( 'NONE',  ( 184.0000000000000568, 17.53993994372673981, -12.49999999999999467 ) ) ;
#14973 = CIRCLE ( 'NONE', #1122, 6.999999999999992006 ) ;
#14974 = LINE ( 'NONE', #12301, #13403 ) ;
#14975 = DIRECTION ( 'NONE',  ( 0.000000000000000000, -1.000000000000000000, 0.000000000000000000 ) ) ;
#14976 = ORIENTED_EDGE ( 'NONE', *, *, #6650, .F. ) ;
#14977 = CARTESIAN_POINT ( 'NONE',  ( -219.0707735969879195, 150.7146073354513476, 9.486927387000964274 ) ) ;
#14978 = VERTEX_POINT ( 'NONE', #11488 ) ;
#14979 = CARTESIAN_POINT ( 'NONE',  ( -167.9381859705957254, 127.3450499201829160, 0.2100378832225609782 ) ) ;
#14980 = LINE ( 'NONE', #13890, #11894 ) ;
#14981 = VERTEX_POINT ( 'NONE', #4206 ) ;
#14982 = CARTESIAN_POINT ( 'NONE',  ( -63.50000000000002842, 15.53993994372673626, 52.49999999999997868 ) ) ;
#14983 = DIRECTION ( 'NONE',  ( 5.518327896226373923E-17, 0.9902680687415712502, 0.1391731009600586100 ) ) ;
#14984 = ADVANCED_FACE ( 'NONE', ( #9043 ), #11319, .T. ) ;
#14985 = VECTOR ( 'NONE', #14166, 1000.000000000000000 ) ;
#14986 = CARTESIAN_POINT ( 'NONE',  ( 177.5000000000000853, -178.8753867012115961, -29.82329228561640022 ) ) ;
#14987 = EDGE_LOOP ( 'NONE', ( #15393, #8975, #4825, #9177 ) ) ;
#14988 = EDGE_CURVE ( 'NONE', #13434, #8877, #10069, .T. ) ;
#14989 = EDGE_CURVE ( 'NONE', #13397, #11374, #13061, .T. ) ;
#14990 = ITEM_DEFINED_TRANSFORMATION ( 'NONE', 'NONE', #8056,  #12337 ) ;
#14991 = ORIENTED_EDGE ( 'NONE', *, *, #12338, .F. ) ;
#14992 = CARTESIAN_POINT ( 'NONE',  ( 209.5385712735872517, 33.62447922832576097, -6.247773722084159154 ) ) ;
#14993 = EDGE_CURVE ( 'NONE', #256, #14924, #10225, .T. ) ;
#14994 = EDGE_CURVE ( 'NONE', #2210, #591, #12729, .T. ) ;
#14995 = CARTESIAN_POINT ( 'NONE',  ( -156.9343249342362583, 111.1640292632437905, 9.769994122432187567 ) ) ;
#14996 = VERTEX_POINT ( 'NONE', #12423 ) ;
#14997 = DIRECTION ( 'NONE',  ( 0.000000000000000000, -1.000000000000000000, -0.000000000000000000 ) ) ;
#14998 = AXIS2_PLACEMENT_3D ( 'NONE', #13904, #11623, #13981 ) ;
#14999 = PLANE ( 'NONE',  #7051 ) ;
#15000 = ORIENTED_EDGE ( 'NONE', *, *, #7569, .F. ) ;
#15001 = ORIENTED_EDGE ( 'NONE', *, *, #13360, .T. ) ;
#15002 = CARTESIAN_POINT ( 'NONE',  ( -169.9318100387881714, 128.7846982781319412, 2.500000000781056997 ) ) ;
#15003 = AXIS2_PLACEMENT_3D ( 'NONE', #3504, #11960, #8342 ) ;
#15004 = DIRECTION ( 'NONE',  ( 1.000000000000000000, 0.000000000000000000, 0.000000000000000000 ) ) ;
#15005 = EDGE_LOOP ( 'NONE', ( #4900, #11854 ) ) ;
#15006 = CARTESIAN_POINT ( 'NONE',  ( 0.000000000000000000, -6.928203230275514990, 4.000000000000058620 ) ) ;
#15007 = DIRECTION ( 'NONE',  ( -0.000000000000000000, -0.000000000000000000, 1.000000000000000000 ) ) ;
#15008 = CARTESIAN_POINT ( 'NONE',  ( -70.00000000000000000, 17.53993994372673981, -12.49999999999999289 ) ) ;
#15009 = CARTESIAN_POINT ( 'NONE',  ( 184.0000000000000568, 17.53993994372673626, 48.99999999999997158 ) ) ;
#15010 = DIRECTION ( 'NONE',  ( -1.000000000000000000, 0.000000000000000000, 0.000000000000000000 ) ) ;
#15011 = AXIS2_PLACEMENT_3D ( 'NONE', #7125, #3143, #12761 ) ;
#15012 = EDGE_CURVE ( 'NONE', #5538, #13816, #8309, .T. ) ;
#15013 = ADVANCED_FACE ( 'NONE', ( #3042 ), #6753, .F. ) ;
#15014 = EDGE_CURVE ( 'NONE', #9239, #8771, #14586, .T. ) ;
#15015 = DIRECTION ( 'NONE',  ( 1.000000000000000000, -2.751328491981765035E-32, 3.965082230804130220E-16 ) ) ;
#15016 = ORIENTED_EDGE ( 'NONE', *, *, #4772, .F. ) ;
#15017 = LINE ( 'NONE', #7869, #6704 ) ;
#15018 = CARTESIAN_POINT ( 'NONE',  ( -188.7806045336324132, 137.2844789098840863, -2.963320117457101777 ) ) ;
#15019 = DIRECTION ( 'NONE',  ( -0.000000000000000000, 1.000000000000000000, -0.000000000000000000 ) ) ;
#15020 = EDGE_LOOP ( 'NONE', ( #1588, #15564 ) ) ;
#15021 = CARTESIAN_POINT ( 'NONE',  ( -218.1518098834511648, 139.2461763302102327, 1.515400478619101987 ) ) ;
#15022 = CARTESIAN_POINT ( 'NONE',  ( 188.3266922173125124, 39.20571348140700252, -7.512715813640810758 ) ) ;
#15023 = VERTEX_POINT ( 'NONE', #11560 ) ;
#15024 = AXIS2_PLACEMENT_3D ( 'NONE', #15449, #4648, #14427 ) ;
#15025 = ADVANCED_FACE ( 'NONE', ( #723 ), #3423, .F. ) ;
#15026 = FACE_BOUND ( 'NONE', #2342, .T. ) ;
#15027 = CARTESIAN_POINT ( 'NONE',  ( -63.50000000000002842, -179.8058001507315566, -17.76585208085566947 ) ) ;
#15028 = CARTESIAN_POINT ( 'NONE',  ( 17.41029453487719181, 40.04259805664093363, 10.00000000000000178 ) ) ;
#15029 = DIRECTION ( 'NONE',  ( 0.000000000000000000, 1.000000000000000000, 0.000000000000000000 ) ) ;
#15030 = VERTEX_POINT ( 'NONE', #9427 ) ;
#15031 = CARTESIAN_POINT ( 'NONE',  ( 122.5806775638430253, 45.00321902537314145, 10.00000000000000178 ) ) ;
#15032 = CARTESIAN_POINT ( 'NONE',  ( -182.2596580518439850, 130.2653702959948987, 9.578254705571840333 ) ) ;
#15033 = CARTESIAN_POINT ( 'NONE',  ( -64.00000000000002842, 15.17911304468679745, 25.93769382960995529 ) ) ;
#15034 = CARTESIAN_POINT ( 'NONE',  ( -156.0423532639127018, 111.0040250659683068, -4.962432776364138043 ) ) ;
#15035 = VERTEX_POINT ( 'NONE', #2316 ) ;
#15036 = CARTESIAN_POINT ( 'NONE',  ( 224.0000000000000853, 22.53993994372673981, 24.99999999999999645 ) ) ;
#15037 = ORIENTED_EDGE ( 'NONE', *, *, #14372, .F. ) ;
#15038 = EDGE_CURVE ( 'NONE', #8632, #15428, #14093, .T. ) ;
#15039 = ORIENTED_EDGE ( 'NONE', *, *, #2911, .F. ) ;
#15040 = DIRECTION ( 'NONE',  ( 1.000000000000000000, 2.751328491981765035E-32, -3.965082230804130220E-16 ) ) ;
#15041 = CARTESIAN_POINT ( 'NONE',  ( 178.0000000000000853, 16.03993994372673981, -17.50000000000002487 ) ) ;
#15042 = CARTESIAN_POINT ( 'NONE',  ( -110.0000000000000426, 56.53993994372675047, 25.00000000000000000 ) ) ;
#15043 = CARTESIAN_POINT ( 'NONE',  ( -168.5655597009508426, 126.2210114011889033, 7.273861828271574126 ) ) ;
#15044 = CARTESIAN_POINT ( 'NONE',  ( -220.4547830239155246, 152.2598634421184727, -4.296684159728658692 ) ) ;
#15045 = CARTESIAN_POINT ( 'NONE',  ( -76.00000000000001421, -179.3058001507315566, -17.76585208085566947 ) ) ;
#15046 = DIRECTION ( 'NONE',  ( 5.518327896226364679E-17, -0.9902680687415713612, 0.1391731009600582492 ) ) ;
#15047 = LINE ( 'NONE', #2994, #15213 ) ;
#15048 = AXIS2_PLACEMENT_3D ( 'NONE', #13159, #10814, #51 ) ;
#15049 = FACE_BOUND ( 'NONE', #2356, .T. ) ;
#15050 = EDGE_CURVE ( 'NONE', #4447, #7175, #6910, .T. ) ;
#15051 = CARTESIAN_POINT ( 'NONE',  ( -219.4169439222603160, 154.1193151060158471, 2.705939130397310599 ) ) ;
#15052 = ORIENTED_EDGE ( 'NONE', *, *, #13357, .F. ) ;
#15053 =( LENGTH_UNIT ( ) NAMED_UNIT ( * ) SI_UNIT ( .MILLI., .METRE. ) );
#15054 = EDGE_LOOP ( 'NONE', ( #14375, #8776, #11139, #15175 ) ) ;
#15055 = ADVANCED_FACE ( 'NONE', ( #6834 ), #7146, .F. ) ;
#15056 = CARTESIAN_POINT ( 'NONE',  ( 0.1306530452038175694, -7.903938623646883599, -2.309976723937606113 ) ) ;
#15057 = CARTESIAN_POINT ( 'NONE',  ( 177.5000000000000853, 19.53993994372674692, -17.50000000000002487 ) ) ;
#15058 = EDGE_LOOP ( 'NONE', ( #6409, #7053 ) ) ;
#15059 = FACE_OUTER_BOUND ( 'NONE', #6184, .T. ) ;
#15060 = DIRECTION ( 'NONE',  ( -0.000000000000000000, 1.000000000000000000, 6.938893903907227145E-17 ) ) ;
#15061 = PRODUCT_DEFINITION_SHAPE ( 'NONE', 'NONE',  #15620 ) ;
#15062 = AXIS2_PLACEMENT_3D ( 'NONE', #12449, #6551, #6472 ) ;
#15063 = CARTESIAN_POINT ( 'NONE',  ( 184.0000000000000568, 19.53993994372674337, -13.99999999999999289 ) ) ;
#15065 = EDGE_LOOP ( 'NONE', ( #189, #1451, #12512, #4838, #9564 ) ) ;
#15064 = ADVANCED_FACE ( 'NONE', ( #4677 ), #14839, .T. ) ;
#15066 = CIRCLE ( 'NONE', #695, 1.499999999999994449 ) ;
#15067 = PRODUCT_CONTEXT ( 'NONE', #3521, 'mechanical' ) ;
#15068 = ORIENTED_EDGE ( 'NONE', *, *, #15288, .T. ) ;
#15069 = CARTESIAN_POINT ( 'NONE',  ( 190.6178699541428898, 33.66405957396897719, -4.118459193090428627 ) ) ;
#15070 = DIRECTION ( 'NONE',  ( -0.4147405137080060755, 0.9099397267342597129, 0.000000000000000000 ) ) ;
#15071 = ORIENTED_EDGE ( 'NONE', *, *, #12063, .F. ) ;
#15072 = DIRECTION ( 'NONE',  ( 1.000000000000000000, 0.000000000000000000, 0.000000000000000000 ) ) ;
#15073 = DIRECTION ( 'NONE',  ( -3.965082230804130220E-16, -0.000000000000000000, -1.000000000000000000 ) ) ;
#15074 = VERTEX_POINT ( 'NONE', #12891 ) ;
#15075 = EDGE_LOOP ( 'NONE', ( #13192, #5135, #4178 ) ) ;
#15076 = DIRECTION ( 'NONE',  ( 0.000000000000000000, -1.000000000000000000, 0.000000000000000000 ) ) ;
#15077 = AXIS2_PLACEMENT_3D ( 'NONE', #5804, #10471, #10625 ) ;
#15078 = DIRECTION ( 'NONE',  ( 1.000000000000000000, 0.000000000000000000, 0.000000000000000000 ) ) ;
#15079 = CIRCLE ( 'NONE', #14573, 1.700000000000007061 ) ;
#15080 = EDGE_CURVE ( 'NONE', #12631, #462, #3769, .T. ) ;
#15081 = ORIENTED_EDGE ( 'NONE', *, *, #747, .T. ) ;
#15082 = CARTESIAN_POINT ( 'NONE',  ( 208.8124460758720033, 42.05191026284237665, -4.433604294307299298 ) ) ;
#15083 = CARTESIAN_POINT ( 'NONE',  ( 10.39230484541326582, 0.000000000000000000, 5.000000000000000000 ) ) ;
#15084 = DIRECTION ( 'NONE',  ( -0.000000000000000000, -0.000000000000000000, 1.000000000000000000 ) ) ;
#15085 = DIRECTION ( 'NONE',  ( 0.000000000000000000, 0.000000000000000000, 1.000000000000000000 ) ) ;
#15086 = DIRECTION ( 'NONE',  ( -0.000000000000000000, -0.000000000000000000, 1.000000000000000000 ) ) ;
#15087 = AXIS2_PLACEMENT_3D ( 'NONE', #3227, #11686, #5607 ) ;
#15088 = AXIS2_PLACEMENT_3D ( 'NONE', #4758, #10929, #84 ) ;
#15089 = FACE_OUTER_BOUND ( 'NONE', #13777, .T. ) ;
#15090 = EDGE_LOOP ( 'NONE', ( #10514, #9756, #4344, #6721 ) ) ;
#15091 = CARTESIAN_POINT ( 'NONE',  ( 174.2293059057019775, 61.25683321636181233, 10.00000000000000178 ) ) ;
#15092 = CARTESIAN_POINT ( 'NONE',  ( -206.2168697392640695, 148.5706983463157940, -0.4547266291960757045 ) ) ;
#15093 = DIRECTION ( 'NONE',  ( -3.965082230804130220E-16, 1.090924371466202084E-47, 1.000000000000000000 ) ) ;
#15094 = ORIENTED_EDGE ( 'NONE', *, *, #3586, .T. ) ;
#15095 = CARTESIAN_POINT ( 'NONE',  ( -221.5581585947747101, 141.9038310245542505, 5.434137442415940988 ) ) ;
#15096 = UNCERTAINTY_MEASURE_WITH_UNIT (LENGTH_MEASURE( 1.000000000000000082E-05 ), #10146, 'distance_accuracy_value', 'NONE');
#15097 = CARTESIAN_POINT ( 'NONE',  ( 211.8964099132376191, 42.41229301046570299, -5.872780407435223893 ) ) ;
#15098 = ORIENTED_EDGE ( 'NONE', *, *, #12028, .F. ) ;
#15099 = ADVANCED_FACE ( 'NONE', ( #4366 ), #11721, .F. ) ;
#15101 = EDGE_CURVE ( 'NONE', #12980, #8626, #13118, .T. ) ;
#15100 = EDGE_CURVE ( 'NONE', #5874, #555, #15482, .T. ) ;
#15102 = CIRCLE ( 'NONE', #9567, 0.5000000000000000000 ) ;
#15103 = DIRECTION ( 'NONE',  ( -0.000000000000000000, -0.9902680687415711391, -0.1391731009600593039 ) ) ;
#15104 = CARTESIAN_POINT ( 'NONE',  ( 0.2456200930618588907, -1.587713240271461546, 2.750000000000000000 ) ) ;
#15105 = DIRECTION ( 'NONE',  ( 0.000000000000000000, -1.000000000000000000, 0.000000000000000000 ) ) ;
#15106 = AXIS2_PLACEMENT_3D ( 'NONE', #13220, #4707, #15430 ) ;
#15107 = DIRECTION ( 'NONE',  ( 0.000000000000000000, 0.000000000000000000, 1.000000000000000000 ) ) ;
#15108 = ORIENTED_EDGE ( 'NONE', *, *, #9556, .T. ) ;
#15109 = AXIS2_PLACEMENT_3D ( 'NONE', #3033, #7864, #14933 ) ;
#15110 = DIRECTION ( 'NONE',  ( 1.000000000000000000, 0.000000000000000000, 0.000000000000000000 ) ) ;
#15111 = CARTESIAN_POINT ( 'NONE',  ( -179.6920193139674780, 128.7453118898713456, 9.578254705571842109 ) ) ;
#15112 = CARTESIAN_POINT ( 'NONE',  ( 164.0000000000000568, 64.53993994372673626, 15.00000000000000355 ) ) ;
#15113 = CYLINDRICAL_SURFACE ( 'NONE', #7315, 1.499999999999997780 ) ;
#15114 = EDGE_LOOP ( 'NONE', ( #1620, #7210 ) ) ;
#15115 = FACE_BOUND ( 'NONE', #9236, .T. ) ;
#15116 = EDGE_LOOP ( 'NONE', ( #4739, #955, #12075, #13609 ) ) ;
#15117 = EDGE_LOOP ( 'NONE', ( #14299, #6663, #8118, #10003 ) ) ;
#15118 = AXIS2_PLACEMENT_3D ( 'NONE', #13671, #2797, #1305 ) ;
#15119 = CARTESIAN_POINT ( 'NONE',  ( -70.00000000000000000, -179.3058001507315566, 76.45141194869098911 ) ) ;
#15120 = CARTESIAN_POINT ( 'NONE',  ( 193.3006371371548369, 56.51400776751751920, 5.000000000000000000 ) ) ;
#15121 = VECTOR ( 'NONE', #4241, 1000.000000000000000 ) ;
#15122 = CIRCLE ( 'NONE', #6833, 4.999999999999990230 ) ;
#15123 = CARTESIAN_POINT ( 'NONE',  ( -76.50000000000002842, 19.53993994372674337, 24.99999999999999645 ) ) ;
#15124 = CARTESIAN_POINT ( 'NONE',  ( -168.3730750733982973, 126.5658778264387507, 6.698921820633309210 ) ) ;
#15125 = CARTESIAN_POINT ( 'NONE',  ( -219.4139989654581768, 154.1245914584070533, 2.346545549012409637 ) ) ;
#15126 = DIRECTION ( 'NONE',  ( 0.000000000000000000, 0.000000000000000000, 1.000000000000000000 ) ) ;
#15127 = CARTESIAN_POINT ( 'NONE',  ( 177.5000000000000853, 19.53993994372674692, -17.50000000000002487 ) ) ;
#15128 = VECTOR ( 'NONE', #3743, 1000.000000000000000 ) ;
#15129 = CARTESIAN_POINT ( 'NONE',  ( 224.0000000000000853, 22.53993994372673981, 13.00000000000000178 ) ) ;
#15130 = AXIS2_PLACEMENT_3D ( 'NONE', #7380, #9820, #14572 ) ;
#15131 = DIRECTION ( 'NONE',  ( 0.000000000000000000, 1.000000000000000000, 8.673617379884035472E-17 ) ) ;
#15132 = EDGE_CURVE ( 'NONE', #11374, #13397, #5535, .T. ) ;
#15133 = CARTESIAN_POINT ( 'NONE',  ( 13.07968152355895874, 460.3807876674321165, 5.000000000000000000 ) ) ;
#15134 = CARTESIAN_POINT ( 'NONE',  ( -219.4360840196855804, 154.0850226169901305, 3.058976617611859794 ) ) ;
#15135 = ORIENTED_EDGE ( 'NONE', *, *, #2424, .T. ) ;
#15136 = ORIENTED_EDGE ( 'NONE', *, *, #11927, .F. ) ;
#15137 = CARTESIAN_POINT ( 'NONE',  ( 174.2293059057019775, 61.25683321636181233, 10.00000000000000178 ) ) ;
#15138 = FACE_OUTER_BOUND ( 'NONE', #9516, .T. ) ;
#15139 = LINE ( 'NONE', #14040, #5108 ) ;
#15140 = CARTESIAN_POINT ( 'NONE',  ( 14.00000000000004086, 64.53993994372673626, 15.00000000000104983 ) ) ;
#15141 = DIRECTION ( 'NONE',  ( 0.000000000000000000, 0.000000000000000000, 1.000000000000000000 ) ) ;
#15142 = AXIS2_PLACEMENT_3D ( 'NONE', #14927, #4119, #13746 ) ;
#15143 = AXIS2_PLACEMENT_3D ( 'NONE', #10097, #1714, #6394 ) ;
#15144 = DIRECTION ( 'NONE',  ( 0.000000000000000000, 0.000000000000000000, 1.000000000000000000 ) ) ;
#15145 = EDGE_LOOP ( 'NONE', ( #4905, #12196, #2146, #5851 ) ) ;
#15146 = ADVANCED_FACE ( 'NONE', ( #11952 ), #11644, .T. ) ;
#15147 = APPLICATION_PROTOCOL_DEFINITION ( 'draft international standard', 'automotive_design', 1998, #3521 ) ;
#15148 = ORIENTED_EDGE ( 'NONE', *, *, #4517, .F. ) ;
#15149 = CARTESIAN_POINT ( 'NONE',  ( 207.2255354594468884, 50.38222520613008015, -5.636003230111601425 ) ) ;
#15150 = VERTEX_POINT ( 'NONE', #3347 ) ;
#15151 = DIRECTION ( 'NONE',  ( 1.000000000000000000, 0.000000000000000000, 0.000000000000000000 ) ) ;
#15152 = TOROIDAL_SURFACE ( 'NONE', #5087, 1.000000000000000000, 0.5000000000000000000 ) ;
#15153 = CARTESIAN_POINT ( 'NONE',  ( -224.6032697205328645, 144.8271983225910162, 2.539373236809186807 ) ) ;
#15154 = ORIENTED_EDGE ( 'NONE', *, *, #6017, .F. ) ;
#15155 = VERTEX_POINT ( 'NONE', #13032 ) ;
#15156 = AXIS2_PLACEMENT_3D ( 'NONE', #7828, #14900, #11368 ) ;
#15157 = CARTESIAN_POINT ( 'NONE',  ( -36.49899788034579018, 48.72489408690345414, 10.00000000000000178 ) ) ;
#15158 = VERTEX_POINT ( 'NONE', #10378 ) ;
#15159 = CARTESIAN_POINT ( 'NONE',  ( 202.9928097691983169, 48.86380790798758511, -0.9029304599467440351 ) ) ;
#15160 = DIRECTION ( 'NONE',  ( -0.000000000000000000, -0.000000000000000000, 1.000000000000000000 ) ) ;
#15161 = CARTESIAN_POINT ( 'NONE',  ( 6.399999999999999467, -9.237604307034018802, 2.775557561562891351E-14 ) ) ;
#15162 = DIRECTION ( 'NONE',  ( 1.000000000000000000, 0.000000000000000000, 0.000000000000000000 ) ) ;
#15163 = FACE_OUTER_BOUND ( 'NONE', #10497, .T. ) ;
#15164 = AXIS2_PLACEMENT_3D ( 'NONE', #10314, #5336, #11572 ) ;
#15165 = AXIS2_PLACEMENT_3D ( 'NONE', #11035, #3771, #187 ) ;
#15166 = EDGE_CURVE ( 'NONE', #9501, #8250, #15171, .T. ) ;
#15167 = CARTESIAN_POINT ( 'NONE',  ( 164.0000000000000568, 64.53993994372673626, 11.47500000000000320 ) ) ;
#15168 = VERTEX_POINT ( 'NONE', #12967 ) ;
#15169 = DIRECTION ( 'NONE',  ( -1.000000000000000000, 0.000000000000000000, 0.000000000000000000 ) ) ;
#15170 = CARTESIAN_POINT ( 'NONE',  ( -206.8675068987516283, 149.4103724542255804, 1.515441477536285220 ) ) ;
#15171 = LINE ( 'NONE', #14073, #9568 ) ;
#15172 = ORIENTED_EDGE ( 'NONE', *, *, #6163, .T. ) ;
#15173 = CARTESIAN_POINT ( 'NONE',  ( -173.0624365063895311, 117.4516868700737433, -3.188270265946634208 ) ) ;
#15174 = CARTESIAN_POINT ( 'NONE',  ( 211.8657363685815653, 42.56416725473636831, -9.010781945348840694 ) ) ;
#15175 = ORIENTED_EDGE ( 'NONE', *, *, #1390, .T. ) ;
#15177 = STYLED_ITEM ( 'NONE', ( #6232 ), #243 ) ;
#15176 = VECTOR ( 'NONE', #12017, 1000.000000000000000 ) ;
#15178 = FACE_BOUND ( 'NONE', #230, .T. ) ;
#15179 = LINE ( 'NONE', #12815, #14508 ) ;
#15180 = EDGE_CURVE ( 'NONE', #10184, #5373, #4769, .T. ) ;
#15181 = CARTESIAN_POINT ( 'NONE',  ( 190.5000000000000568, 16.03993994372673981, 10.05257423913146475 ) ) ;
#15182 = CARTESIAN_POINT ( 'NONE',  ( 0.000000000000000000, 0.000000000000000000, 0.000000000000000000 ) ) ;
#15183 = DIRECTION ( 'NONE',  ( -3.965082230804130220E-16, 1.090924371466202084E-47, 1.000000000000000000 ) ) ;
#15184 = ADVANCED_FACE ( 'NONE', ( #2154 ), #962, .T. ) ;
#15185 = ADVANCED_FACE ( 'NONE', ( #15247 ), #4442, .F. ) ;
#15186 = AXIS2_PLACEMENT_3D ( 'NONE', #5458, #12630, #6802 ) ;
#15187 = EDGE_LOOP ( 'NONE', ( #10601, #8313, #11804, #7195 ) ) ;
#15188 = CARTESIAN_POINT ( 'NONE',  ( -34.79899788034579444, 48.72489408690345414, 10.00000000000000178 ) ) ;
#15189 = CARTESIAN_POINT ( 'NONE',  ( -220.8021227237918254, 143.2564083082033619, 7.918248976830615682 ) ) ;
#15190 = DIRECTION ( 'NONE',  ( -0.4873681696970831312, -0.8731965799097676229, 0.000000000000000000 ) ) ;
#15191 = EDGE_CURVE ( 'NONE', #1434, #15197, #9741, .T. ) ;
#15192 = DIRECTION ( 'NONE',  ( -0.000000000000000000, 1.000000000000000000, 0.000000000000000000 ) ) ;
#15193 = VERTEX_POINT ( 'NONE', #12174 ) ;
#15194 = CARTESIAN_POINT ( 'NONE',  ( -76.50000000000004263, -178.8058001507315566, 52.19066787724494816 ) ) ;
#15195 = PRESENTATION_LAYER_ASSIGNMENT (  '', '', ( #13443 ) ) ;
#15196 = ORIENTED_EDGE ( 'NONE', *, *, #7340, .F. ) ;
#15197 = VERTEX_POINT ( 'NONE', #1277 ) ;
#15198 = CYLINDRICAL_SURFACE ( 'NONE', #15366, 0.5000000000000004441 ) ;
#15199 = LINE ( 'NONE', #15120, #12049 ) ;
#15200 = DIRECTION ( 'NONE',  ( 0.000000000000000000, 0.000000000000000000, -1.000000000000000000 ) ) ;
#15201 = CARTESIAN_POINT ( 'NONE',  ( -168.8600800343791377, 125.6933319919581464, 7.985209213891318214 ) ) ;
#15202 = CARTESIAN_POINT ( 'NONE',  ( -222.5547230352208032, 144.0789707147005458, -3.043139129519528030 ) ) ;
#15203 = VECTOR ( 'NONE', #2607, 1000.000000000000000 ) ;
#15204 = DIRECTION ( 'NONE',  ( -1.000000000000000000, -0.000000000000000000, -0.000000000000000000 ) ) ;
#15205 = EDGE_CURVE ( 'NONE', #10763, #4290, #2393, .T. ) ;
#15206 = CIRCLE ( 'NONE', #10439, 1.000000000000000888 ) ;
#15207 = EDGE_CURVE ( 'NONE', #11977, #3709, #8813, .T. ) ;
#15208 = CARTESIAN_POINT ( 'NONE',  ( 191.8042410000843745, 59.95507574834591225, 5.000000000000000000 ) ) ;
#15209 = LINE ( 'NONE', #15129, #13695 ) ;
#15210 = CARTESIAN_POINT ( 'NONE',  ( 73.79035645333922844, 38.79159067395544014, 10.00000000000000178 ) ) ;
#15211 = CARTESIAN_POINT ( 'NONE',  ( -224.1994838848473250, 145.5506440309058860, -0.5027386702675625818 ) ) ;
#15212 = VERTEX_POINT ( 'NONE', #3890 ) ;
#15213 = VECTOR ( 'NONE', #9163, 1000.000000000000000 ) ;
#15214 = SHAPE_REPRESENTATION_RELATIONSHIP ( 'NONE' , 'NONE' ,  #3806, #6418 ) ;
#15215 = EDGE_LOOP ( 'NONE', ( #2011, #12989, #6032 ) ) ;
#15216 = CARTESIAN_POINT ( 'NONE',  ( 178.0000000000000853, 15.03993994372673804, 24.94742576086838781 ) ) ;
#15217 = DIRECTION ( 'NONE',  ( 1.000000000000000000, 0.000000000000000000, 0.000000000000000000 ) ) ;
#15218 = VERTEX_POINT ( 'NONE', #2708 ) ;
#15219 = CARTESIAN_POINT ( 'NONE',  ( -206.8718859864436581, 149.4025266312245037, 2.500000000000000000 ) ) ;
#15220 = LINE ( 'NONE', #10581, #3802 ) ;
#15221 = ADVANCED_FACE ( 'NONE', ( #9900 ), #4845, .F. ) ;
#15222 = DIRECTION ( 'NONE',  ( 0.000000000000000000, -1.000000000000000000, -1.486905836551548832E-16 ) ) ;
#15223 = ORIENTED_EDGE ( 'NONE', *, *, #13565, .F. ) ;
#15224 = AXIS2_PLACEMENT_3D ( 'NONE', #14184, #10495, #2115 ) ;
#15225 = ORIENTED_EDGE ( 'NONE', *, *, #9721, .F. ) ;
#15226 = CARTESIAN_POINT ( 'NONE',  ( 201.8412736707888087, 29.11599755995149152, -3.759251452247287517 ) ) ;
#15227 = SURFACE_STYLE_FILL_AREA ( #5618 ) ;
#15228 = ORIENTED_EDGE ( 'NONE', *, *, #10764, .T. ) ;
#15229 = LINE ( 'NONE', #4421, #5185 ) ;
#15230 = ORIENTED_EDGE ( 'NONE', *, *, #12782, .T. ) ;
#15231 = ORIENTED_EDGE ( 'NONE', *, *, #10642, .F. ) ;
#15232 = DIRECTION ( 'NONE',  ( 2.751328491981765035E-32, 1.000000000000000000, 1.090924371466202084E-47 ) ) ;
#15233 = CARTESIAN_POINT ( 'NONE',  ( 178.0000000000000853, -179.3058001507315566, 84.88378295107887084 ) ) ;
#15234 = CIRCLE ( 'NONE', #7955, 0.5000000000000004441 ) ;
#15235 = VERTEX_POINT ( 'NONE', #7300 ) ;
#15236 = B_SPLINE_CURVE_WITH_KNOTS ( 'NONE', 3,
 ( #4717, #3459, #924, #9539, #7026, #13075 ),
 .UNSPECIFIED., .F., .F.,
 ( 4, 2, 4 ),
 ( 0.001606744326298693154, 0.002406996759593252669, 0.003207249192887813051 ),
 .UNSPECIFIED. ) ;
#15237 = DIRECTION ( 'NONE',  ( -0.000000000000000000, 1.000000000000000000, -0.000000000000000000 ) ) ;
#15238 = EDGE_CURVE ( 'NONE', #2617, #12412, #9663, .T. ) ;
#15239 = CARTESIAN_POINT ( 'NONE',  ( -110.0000000000000426, 59.53993994372674337, 25.00000000000000000 ) ) ;
#15240 = DIRECTION ( 'NONE',  ( -0.000000000000000000, 1.000000000000000000, 1.156482317317871725E-16 ) ) ;
#15241 = DIRECTION ( 'NONE',  ( 0.000000000000000000, 0.000000000000000000, -1.000000000000000000 ) ) ;
#15242 = AXIS2_PLACEMENT_3D ( 'NONE', #14378, #9660, #5713 ) ;
#15243 = PLANE ( 'NONE',  #1242 ) ;
#15244 = FACE_OUTER_BOUND ( 'NONE', #5652, .T. ) ;
#15245 = CARTESIAN_POINT ( 'NONE',  ( -211.4625087271040513, 151.5689812133889234, -0.4547266291960755935 ) ) ;
#15246 = EDGE_CURVE ( 'NONE', #14091, #8424, #9324, .T. ) ;
#15247 = FACE_OUTER_BOUND ( 'NONE', #3402, .T. ) ;
#15248 = ORIENTED_EDGE ( 'NONE', *, *, #11565, .F. ) ;
#15249 = CARTESIAN_POINT ( 'NONE',  ( -210.8320337336493822, 142.3623933791497791, -5.230826428279598872 ) ) ;
#15250 = CARTESIAN_POINT ( 'NONE',  ( 207.5020891771285960, 50.23084475345794431, 0.4952462535581279024 ) ) ;
#15251 = ORIENTED_EDGE ( 'NONE', *, *, #9805, .F. ) ;
#15252 = DIRECTION ( 'NONE',  ( -0.3662838836490107108, 0.9305003370641705684, 0.002288952263120965468 ) ) ;
#15253 = DIRECTION ( 'NONE',  ( -0.4999999999999997224, -0.8660254037844388186, 0.000000000000000000 ) ) ;
#15254 = EDGE_CURVE ( 'NONE', #5209, #2490, #14458, .T. ) ;
#15255 = CIRCLE ( 'NONE', #3679, 1.000000000000000888 ) ;
#15256 = DIRECTION ( 'NONE',  ( 0.000000000000000000, -6.938893903907227145E-17, 1.000000000000000000 ) ) ;
#15257 = VERTEX_POINT ( 'NONE', #8557 ) ;
#15258 = SHAPE_REPRESENTATION_RELATIONSHIP ( 'NONE' , 'NONE' ,  #3387, #15616 ) ;
#15259 = DIRECTION ( 'NONE',  ( 1.000000000000000000, 0.000000000000000000, 0.000000000000000000 ) ) ;
#15260 = ORIENTED_EDGE ( 'NONE', *, *, #4301, .T. ) ;
#15261 = CARTESIAN_POINT ( 'NONE',  ( -157.8787660911425803, 118.6941998492684149, 5.000000000000000000 ) ) ;
#15262 = CARTESIAN_POINT ( 'NONE',  ( -170.8670245162619779, 127.1065088405712373, 7.890326795182211583 ) ) ;
#15263 = LINE ( 'NONE', #9520, #13811 ) ;
#15264 = CARTESIAN_POINT ( 'NONE',  ( -64.00000000000002842, -179.8058001507315566, 52.49999999999997868 ) ) ;
#15265 = ORIENTED_EDGE ( 'NONE', *, *, #12696, .F. ) ;
#15266 = AXIS2_PLACEMENT_3D ( 'NONE', #9116, #4275, #12563 ) ;
#15267 = CARTESIAN_POINT ( 'NONE',  ( 10.39230484541326582, 0.000000000000000000, 5.000000000000000000 ) ) ;
#15268 = AXIS2_PLACEMENT_3D ( 'NONE', #13063, #10007, #7560 ) ;
#15269 = ORIENTED_EDGE ( 'NONE', *, *, #1267, .F. ) ;
#15270 = ORIENTED_EDGE ( 'NONE', *, *, #335, .T. ) ;
#15271 = CARTESIAN_POINT ( 'NONE',  ( 64.00000000000005684, 59.53993994372674337, 15.00000000000070166 ) ) ;
#15272 = DIRECTION ( 'NONE',  ( 0.000000000000000000, 0.1391731009600626345, 0.9902680687415706950 ) ) ;
#15273 = EDGE_CURVE ( 'NONE', #6329, #3093, #10539, .T. ) ;
#15274 = CARTESIAN_POINT ( 'NONE',  ( -63.50000000000002842, 16.03993994372673626, 38.07518420361041933 ) ) ;
#15275 = CARTESIAN_POINT ( 'NONE',  ( -172.3086228175700398, 119.5147262659699265, 9.219235224006146368 ) ) ;
#15276 = CARTESIAN_POINT ( 'NONE',  ( -223.8857310410845969, 146.1127815013952898, -1.344505601181561927 ) ) ;
#15277 = CARTESIAN_POINT ( 'NONE',  ( 15.71029453487719074, 40.04259805664093363, 7.600000000000002309 ) ) ;
#15278 = DIRECTION ( 'NONE',  ( 1.000000000000000000, 0.000000000000000000, 0.000000000000000000 ) ) ;
#15279 = PRODUCT_DEFINITION_CONTEXT ( 'detailed design', #10193, 'design' ) ;
#15280 = DIRECTION ( 'NONE',  ( -1.000000000000000000, -0.000000000000000000, -0.000000000000000000 ) ) ;
#15281 = DIRECTION ( 'NONE',  ( 0.000000000000000000, 8.673617379884035472E-17, -1.000000000000000000 ) ) ;
#15282 = DIRECTION ( 'NONE',  ( 0.000000000000000000, -1.000000000000000000, 0.000000000000000000 ) ) ;
#15283 = EDGE_LOOP ( 'NONE', ( #12676, #2999 ) ) ;
#15284 =( LENGTH_UNIT ( ) NAMED_UNIT ( * ) SI_UNIT ( .MILLI., .METRE. ) );
#15285 = ORIENTED_EDGE ( 'NONE', *, *, #2223, .F. ) ;
#15286 = CARTESIAN_POINT ( 'NONE',  ( 190.0000000000000853, 15.10952649420676686, 25.44255979523916977 ) ) ;
#15287 = CARTESIAN_POINT ( 'NONE',  ( 164.0000000000000568, 64.53993994372673626, 18.52500000000000213 ) ) ;
#15288 = EDGE_CURVE ( 'NONE', #6079, #1572, #4010, .T. ) ;
#15289 = EDGE_LOOP ( 'NONE', ( #1689, #5320, #2197 ) ) ;
#15290 = EDGE_CURVE ( 'NONE', #8972, #12197, #12831, .T. ) ;
#15291 = DIRECTION ( 'NONE',  ( 0.000000000000000000, 1.000000000000000000, 0.000000000000000000 ) ) ;
#15292 = DIRECTION ( 'NONE',  ( 0.000000000000000000, 0.000000000000000000, -1.000000000000000000 ) ) ;
#15293 = EDGE_CURVE ( 'NONE', #3314, #4062, #4252, .T. ) ;
#15294 = DIRECTION ( 'NONE',  ( -1.000000000000000000, 0.000000000000000000, 0.000000000000000000 ) ) ;
#15295 = EDGE_LOOP ( 'NONE', ( #13131, #4705 ) ) ;
#15296 = AXIS2_PLACEMENT_3D ( 'NONE', #6583, #12550, #14686 ) ;
#15297 = ORIENTED_EDGE ( 'NONE', *, *, #10235, .F. ) ;
#15298 = CARTESIAN_POINT ( 'NONE',  ( 201.7245916543302826, 29.07256658421868423, -6.764440628860102223 ) ) ;
#15299 = LINE ( 'NONE', #939, #2827 ) ;
#15300 = ORIENTED_EDGE ( 'NONE', *, *, #4911, .F. ) ;
#15301 = DIRECTION ( 'NONE',  ( 0.000000000000000000, 0.000000000000000000, -1.000000000000000000 ) ) ;
#15302 = CARTESIAN_POINT ( 'NONE',  ( -76.50000000000004263, 15.53993994372673626, 52.49999999999997868 ) ) ;
#15303 = APPLICATION_CONTEXT ( 'automotive_design' ) ;
#15304 = FACE_BOUND ( 'NONE', #4265, .T. ) ;
#15305 = ORIENTED_EDGE ( 'NONE', *, *, #2284, .F. ) ;
#15306 = VERTEX_POINT ( 'NONE', #8414 ) ;
#15307 = CARTESIAN_POINT ( 'NONE',  ( -144.0627431139473345, 95.36268816863731956, 5.000000000000000000 ) ) ;
#15308 = DIRECTION ( 'NONE',  ( 0.000000000000000000, -1.000000000000000000, 0.000000000000000000 ) ) ;
#15309 = EDGE_LOOP ( 'NONE', ( #7375, #5682, #12250, #2691 ) ) ;
#15310 = AXIS2_PLACEMENT_3D ( 'NONE', #15041, #13788, #2023 ) ;
#15311 = FACE_OUTER_BOUND ( 'NONE', #7448, .T. ) ;
#15312 = DIRECTION ( 'NONE',  ( -0.000000000000000000, 1.000000000000000000, -0.000000000000000000 ) ) ;
#15313 = AXIS2_PLACEMENT_3D ( 'NONE', #272, #2592, #186 ) ;
#15314 = FACE_OUTER_BOUND ( 'NONE', #14164, .T. ) ;
#15315 = PRODUCT_DEFINITION_SHAPE ( 'NONE', 'NONE',  #15622 ) ;
#15316 = CIRCLE ( 'NONE', #8544, 1.499999999999994449 ) ;
#15317 = FILL_AREA_STYLE ('',( #2149 ) ) ;
#15318 = ADVANCED_FACE ( 'NONE', ( #8635 ), #11080, .T. ) ;
#15319 = AXIS2_PLACEMENT_3D ( 'NONE', #8778, #226, #2329 ) ;
#15320 = ORIENTED_EDGE ( 'NONE', *, *, #7394, .F. ) ;
#15321 = DIRECTION ( 'NONE',  ( -0.000000000000000000, -0.000000000000000000, 1.000000000000000000 ) ) ;
#15322 = EDGE_CURVE ( 'NONE', #12236, #9639, #12604, .T. ) ;
#15323 = CARTESIAN_POINT ( 'NONE',  ( -70.00000000000000000, -201.3058001507315566, -39.95141194869120937 ) ) ;
#15324 = DIRECTION ( 'NONE',  ( 0.6130913241491352528, 0.7900120431063440973, -6.390853288732736916E-17 ) ) ;
#15325 = ORIENTED_EDGE ( 'NONE', *, *, #2663, .F. ) ;
#15326 = CARTESIAN_POINT ( 'NONE',  ( -179.8633755235878198, 122.3938961877832696, -4.689260562946571120 ) ) ;
#15327 = CARTESIAN_POINT ( 'NONE',  ( 209.5657782771801578, 33.68426770849990959, -3.244931658323684687 ) ) ;
#15328 = ORIENTED_EDGE ( 'NONE', *, *, #15207, .F. ) ;
#15329 = DIRECTION ( 'NONE',  ( 0.000000000000000000, 0.000000000000000000, 1.000000000000000000 ) ) ;
#15330 = CARTESIAN_POINT ( 'NONE',  ( -76.00000000000001421, 11.87216911405867670, 8.597545510065431884 ) ) ;
#15331 = VECTOR ( 'NONE', #9392, 1000.000000000000000 ) ;
#15332 = DIRECTION ( 'NONE',  ( -1.000000000000000000, -2.751328491981765035E-32, 3.965082230804130220E-16 ) ) ;
#15333 = AXIS2_PLACEMENT_3D ( 'NONE', #9999, #4865, #10872 ) ;
#15334 = ORIENTED_EDGE ( 'NONE', *, *, #13550, .F. ) ;
#15335 = DIRECTION ( 'NONE',  ( 0.000000000000000000, 0.000000000000000000, -1.000000000000000000 ) ) ;
#15336 = EDGE_CURVE ( 'NONE', #11925, #6214, #10075, .T. ) ;
#15337 = CARTESIAN_POINT ( 'NONE',  ( 193.1436046380909772, 46.22450523326372007, -4.738359826975481859 ) ) ;
#15338 = ORIENTED_EDGE ( 'NONE', *, *, #9467, .T. ) ;
#15339 = CYLINDRICAL_SURFACE ( 'NONE', #1365, 1.500000000000001332 ) ;
#15340 = CARTESIAN_POINT ( 'NONE',  ( -224.7572118800429735, 144.5513867789856022, 7.859965607560822853 ) ) ;
#15341 = VECTOR ( 'NONE', #812, 1000.000000000000000 ) ;
#15342 = CARTESIAN_POINT ( 'NONE',  ( -85.99999999999994316, 64.53993994372673626, 15.00000000000174794 ) ) ;
#15343 = CARTESIAN_POINT ( 'NONE',  ( -5.000000000000000000, 0.000000000000000000, 0.000000000000000000 ) ) ;
#15344 = DIRECTION ( 'NONE',  ( -0.000000000000000000, -0.000000000000000000, -1.000000000000000000 ) ) ;
#15345 = ORIENTED_EDGE ( 'NONE', *, *, #164, .T. ) ;
#15346 = ORIENTED_EDGE ( 'NONE', *, *, #6005, .F. ) ;
#15347 = CARTESIAN_POINT ( 'NONE',  ( 190.5000000000000568, -179.3058001507315566, 84.88378295107887084 ) ) ;
#15348 = DIRECTION ( 'NONE',  ( -3.965082230804130220E-16, 4.956352788505162775E-17, -1.000000000000000000 ) ) ;
#15349 = ADVANCED_FACE ( 'NONE', ( #6586 ), #2788, .T. ) ;
#15350 = DIRECTION ( 'NONE',  ( -0.000000000000000000, 1.000000000000000000, -0.000000000000000000 ) ) ;
#15351 = CARTESIAN_POINT ( 'NONE',  ( -171.6707776135659174, 120.6575260737504180, 9.685254691063745369 ) ) ;
#15352 = CARTESIAN_POINT ( 'NONE',  ( -221.8281913388289013, 149.7991868573274985, -5.066262527848913955 ) ) ;
#15353 = AXIS2_PLACEMENT_3D ( 'NONE', #7061, #879, #9423 ) ;
#15354 = VECTOR ( 'NONE', #198, 1000.000000000000000 ) ;
#15355 = ADVANCED_FACE ( 'NONE', ( #388, #6667 ), #14999, .F. ) ;
#15356 = DIRECTION ( 'NONE',  ( 0.000000000000000000, 0.000000000000000000, 1.000000000000000000 ) ) ;
#15357 = DIRECTION ( 'NONE',  ( 1.000000000000000000, -2.751328491981765035E-32, 3.965082230804130220E-16 ) ) ;
#15358 = DIRECTION ( 'NONE',  ( 1.000000000000000000, 0.000000000000000000, 0.000000000000000000 ) ) ;
#15359 = DIRECTION ( 'NONE',  ( 0.000000000000000000, -0.1391731009600591096, 0.9902680687415711391 ) ) ;
#15360 = EDGE_CURVE ( 'NONE', #2732, #14981, #11831, .T. ) ;
#15361 = DIRECTION ( 'NONE',  ( 1.000000000000000000, 0.000000000000000000, 0.000000000000000000 ) ) ;
#15362 = CARTESIAN_POINT ( 'NONE',  ( 51.39999999999999858, 5.616230220889761452E-16, -4.171999999999999709 ) ) ;
#15363 = AXIS2_PLACEMENT_3D ( 'NONE', #9032, #13383, #1754 ) ;
#15364 = LINE ( 'NONE', #3855, #3573 ) ;
#15365 = EDGE_LOOP ( 'NONE', ( #14019, #12445, #5422, #6466, #4439, #3892 ) ) ;
#15366 = AXIS2_PLACEMENT_3D ( 'NONE', #12918, #4551, #8046 ) ;
#15367 = VECTOR ( 'NONE', #10800, 999.9999999999998863 ) ;
#15368 = VERTEX_POINT ( 'NONE', #10278 ) ;
#15369 = CARTESIAN_POINT ( 'NONE',  ( -174.1824175338263387, 116.1575288956428409, 0.3248046258198108993 ) ) ;
#15370 = CARTESIAN_POINT ( 'NONE',  ( -85.99999999999994316, 56.53993994372675047, 13.30000000000175575 ) ) ;
#15371 = ORIENTED_EDGE ( 'NONE', *, *, #7094, .T. ) ;
#15372 = DIRECTION ( 'NONE',  ( -0.000000000000000000, 1.000000000000000000, -0.000000000000000000 ) ) ;
#15373 = DIRECTION ( 'NONE',  ( 0.6130913241491352528, 0.7900120431063439863, -6.390853288732736916E-17 ) ) ;
#15374 = VECTOR ( 'NONE', #4488, 999.9999999999998863 ) ;
#15376 = ORIENTED_EDGE ( 'NONE', *, *, #11267, .T. ) ;
#15375 = EDGE_CURVE ( 'NONE', #4912, #2296, #13335, .T. ) ;
#15377 = CIRCLE ( 'NONE', #6592, 0.5000000000000004441 ) ;
#15378 = CONTEXT_DEPENDENT_SHAPE_REPRESENTATION ( #6463, #8304 ) ;
#15379 = ORIENTED_EDGE ( 'NONE', *, *, #12284, .F. ) ;
#15381 = EDGE_CURVE ( 'NONE', #3488, #9726, #10049, .T. ) ;
#15380 = PRODUCT_DEFINITION ( 'UNKNOWN', '', #8307, #438 ) ;
#15382 = EDGE_CURVE ( 'NONE', #3829, #10747, #3020, .T. ) ;
#15383 = DIRECTION ( 'NONE',  ( -0.000000000000000000, -0.000000000000000000, 1.000000000000000000 ) ) ;
#15384 = EDGE_LOOP ( 'NONE', ( #13898, #5614, #8540, #6803 ) ) ;
#15385 = PLANE ( 'NONE',  #13245 ) ;
#15386 = DIRECTION ( 'NONE',  ( 1.000000000000000000, 0.000000000000000000, 0.000000000000000000 ) ) ;
#15387 = ORIENTED_EDGE ( 'NONE', *, *, #4376, .T. ) ;
#15388 = EDGE_CURVE ( 'NONE', #12671, #13452, #10583, .T. ) ;
#15389 = ORIENTED_EDGE ( 'NONE', *, *, #9891, .F. ) ;
#15390 = CYLINDRICAL_SURFACE ( 'NONE', #3741, 0.5000000000000004441 ) ;
#15391 = CARTESIAN_POINT ( 'NONE',  ( 164.0000000000000568, 56.53993994372675047, 15.00000000000000355 ) ) ;
#15392 = VECTOR ( 'NONE', #1904, 1000.000000000000000 ) ;
#15393 = ORIENTED_EDGE ( 'NONE', *, *, #3533, .F. ) ;
#15394 = DIRECTION ( 'NONE',  ( 0.000000000000000000, 0.1391731009600660485, -0.9902680687415702510 ) ) ;
#15395 = DIRECTION ( 'NONE',  ( 1.000000000000000000, 0.000000000000000000, 0.000000000000000000 ) ) ;
#15396 = VECTOR ( 'NONE', #15445, 1000.000000000000000 ) ;
#15397 = ORIENTED_EDGE ( 'NONE', *, *, #6049, .T. ) ;
#15398 = EDGE_CURVE ( 'NONE', #2407, #815, #2945, .T. ) ;
#15399 = CARTESIAN_POINT ( 'NONE',  ( -76.00000000000004263, -179.3058001507316419, 52.76585208085545986 ) ) ;
#15400 = AXIS2_PLACEMENT_3D ( 'NONE', #14397, #9915, #11017 ) ;
#15401 = ORIENTED_EDGE ( 'NONE', *, *, #4891, .T. ) ;
#15402 = DIRECTION ( 'NONE',  ( 1.000000000000000000, 0.000000000000000000, 0.000000000000000000 ) ) ;
#15403 = CARTESIAN_POINT ( 'NONE',  ( -179.9267697467775520, 134.3633106217456543, 2.500000000000000000 ) ) ;
#15404 = DIRECTION ( 'NONE',  ( 1.000000000000000000, 0.000000000000000000, 0.000000000000000000 ) ) ;
#15405 = ORIENTED_EDGE ( 'NONE', *, *, #8548, .T. ) ;
#15406 = CARTESIAN_POINT ( 'NONE',  ( -214.7080733591933779, 145.5905563435376848, -5.230826428279589990 ) ) ;
#15407 = CARTESIAN_POINT ( 'NONE',  ( 208.8010691282704840, 42.12517885095529380, -3.002821972062079681 ) ) ;
#15408 = ADVANCED_FACE ( 'NONE', ( #4263 ), #3959, .F. ) ;
#15409 = VERTEX_POINT ( 'NONE', #12479 ) ;
#15410 = VECTOR ( 'NONE', #20, 1000.000000000000000 ) ;
#15411 = CARTESIAN_POINT ( 'NONE',  ( 0.02351960456806117053, 2.650883748492876446, 0.9085346626517036839 ) ) ;
#15412 = FACE_BOUND ( 'NONE', #5884, .T. ) ;
#15413 = VECTOR ( 'NONE', #5909, 1000.000000000000000 ) ;
#15414 = CARTESIAN_POINT ( 'NONE',  ( -151.5195349256774762, 106.2703939966685027, -4.358407942927359002 ) ) ;
#15415 = EDGE_CURVE ( 'NONE', #2912, #12821, #5776, .T. ) ;
#15416 = EDGE_LOOP ( 'NONE', ( #5567, #12124, #13598, #3112 ) ) ;
#15417 = ADVANCED_BREP_SHAPE_REPRESENTATION ( '', ( #5438, #10819, #12337 ), #180 ) ;
#15418 = FACE_OUTER_BOUND ( 'NONE', #1901, .T. ) ;
#15419 = ORIENTED_EDGE ( 'NONE', *, *, #12224, .T. ) ;
#15420 = CARTESIAN_POINT ( 'NONE',  ( 177.5000000000000853, 17.53993994372673271, 52.49999999999997868 ) ) ;
#15421 = CARTESIAN_POINT ( 'NONE',  ( -218.1518098834511648, 139.2461763302102327, 1.515400478619101987 ) ) ;
#15422 = LINE ( 'NONE', #13135, #10556 ) ;
#15423 = DIRECTION ( 'NONE',  ( 0.000000000000000000, 0.000000000000000000, -1.000000000000000000 ) ) ;
#15425 = AXIS2_PLACEMENT_3D ( 'NONE', #9783, #5914, #4810 ) ;
#15424 = CONICAL_SURFACE ( 'NONE', #4598, 2.749999999999999112, 1.047197551196600296 ) ;
#15426 = CARTESIAN_POINT ( 'NONE',  ( -76.50000000000004263, -179.8058001507315566, 52.76585208085545275 ) ) ;
#15427 = ORIENTED_EDGE ( 'NONE', *, *, #9080, .T. ) ;
#15428 = VERTEX_POINT ( 'NONE', #12638 ) ;
#15429 = CARTESIAN_POINT ( 'NONE',  ( 190.0000000000000568, 15.17911304468679923, 9.062306170389897275 ) ) ;
#15430 = DIRECTION ( 'NONE',  ( 0.000000000000000000, -1.000000000000000000, -6.938893903907227145E-17 ) ) ;
#15431 = CYLINDRICAL_SURFACE ( 'NONE', #73, 0.4999999999999996114 ) ;
#15432 = DIRECTION ( 'NONE',  ( 0.000000000000000000, 0.000000000000000000, 1.000000000000000000 ) ) ;
#15433 = CARTESIAN_POINT ( 'NONE',  ( -219.6164868915797967, 149.6803330067249931, -4.932213728819581533 ) ) ;
#15434 = ADVANCED_FACE ( 'NONE', ( #7613, #12407 ), #1591, .F. ) ;
#15435 = CARTESIAN_POINT ( 'NONE',  ( -222.1184893299650298, 144.9908166140801882, 8.775148900260887785 ) ) ;
#15436 = VECTOR ( 'NONE', #14888, 1000.000000000000000 ) ;
#15437 = CARTESIAN_POINT ( 'NONE',  ( 164.0000000000000568, 62.13993994372673768, 15.00000000000000355 ) ) ;
#15438 = CARTESIAN_POINT ( 'NONE',  ( 14.00000000000004086, 64.53993994372673626, 13.30000000000105231 ) ) ;
#15439 = CYLINDRICAL_SURFACE ( 'NONE', #1253, 1.700000000000001954 ) ;
#15440 = CARTESIAN_POINT ( 'NONE',  ( 190.0000000000000568, 15.03993994372673804, 24.94742576086838781 ) ) ;
#15441 = CARTESIAN_POINT ( 'NONE',  ( 17.41029453487719181, 40.04259805664093363, 10.00000000000000178 ) ) ;
#15442 = ORIENTED_EDGE ( 'NONE', *, *, #2656, .F. ) ;
#15443 = ORIENTED_EDGE ( 'NONE', *, *, #1290, .F. ) ;
#15444 = CARTESIAN_POINT ( 'NONE',  ( -76.00000000000004263, -179.8058001507315566, 84.88378295107887084 ) ) ;
#15445 = DIRECTION ( 'NONE',  ( -0.4147405137080060755, 0.9099397267342597129, 0.000000000000000000 ) ) ;
#15446 = AXIS2_PLACEMENT_3D ( 'NONE', #14102, #7973, #4236 ) ;
#15447 = DIRECTION ( 'NONE',  ( 0.000000000000000000, 0.000000000000000000, 1.000000000000000000 ) ) ;
#15448 = CARTESIAN_POINT ( 'NONE',  ( -174.7846310273254176, 131.4932641812416421, 2.500000000270498735 ) ) ;
#15449 = CARTESIAN_POINT ( 'NONE',  ( 184.0000000000000568, -181.3058001507315566, 76.45141194869098911 ) ) ;
#15450 = PRODUCT ( 'MAS-307', 'MAS-307', '', ( #6420 ) ) ;
#15451 = EDGE_CURVE ( 'NONE', #1469, #13988, #13073, .T. ) ;
#15452 = PRESENTATION_LAYER_ASSIGNMENT (  '', '', ( #11186 ) ) ;
#15453 = ADVANCED_FACE ( 'NONE', ( #2869 ), #8872, .T. ) ;
#15454 = ORIENTED_EDGE ( 'NONE', *, *, #9952, .T. ) ;
#15455 = CONTEXT_DEPENDENT_SHAPE_REPRESENTATION ( #12392, #13807 ) ;
#15456 = ORIENTED_EDGE ( 'NONE', *, *, #14312, .F. ) ;
#15457 = AXIS2_PLACEMENT_3D ( 'NONE', #344, #14564, #5183 ) ;
#15458 = CARTESIAN_POINT ( 'NONE',  ( 204.2383844621755884, 51.59388984732451888, -2.501575441055724713 ) ) ;
#15459 = CARTESIAN_POINT ( 'NONE',  ( 190.0000000000000568, -179.8058001507315566, -17.50000000000002487 ) ) ;
#15460 = ORIENTED_EDGE ( 'NONE', *, *, #14870, .T. ) ;
#15461 = DIRECTION ( 'NONE',  ( -1.000000000000000000, 0.000000000000000000, 0.000000000000000000 ) ) ;
#15462 = CIRCLE ( 'NONE', #2881, 3.500000000000003109 ) ;
#15463 = PLANE ( 'NONE',  #7345 ) ;
#15464 = DIRECTION ( 'NONE',  ( -0.000000000000000000, -0.000000000000000000, 1.000000000000000000 ) ) ;
#15465 = ORIENTED_EDGE ( 'NONE', *, *, #9364, .F. ) ;
#15466 = ORIENTED_EDGE ( 'NONE', *, *, #13914, .T. ) ;
#15467 = DIRECTION ( 'NONE',  ( 0.000000000000000000, 4.956352788505162775E-17, -1.000000000000000000 ) ) ;
#15468 = ADVANCED_FACE ( 'NONE', ( #7765 ), #12299, .F. ) ;
#15469 = DIRECTION ( 'NONE',  ( 0.000000000000000000, 0.000000000000000000, -1.000000000000000000 ) ) ;
#15470 = EDGE_LOOP ( 'NONE', ( #13209, #2037 ) ) ;
#15471 = PLANE ( 'NONE',  #11553 ) ;
#15472 = FACE_BOUND ( 'NONE', #6351, .T. ) ;
#15473 = CIRCLE ( 'NONE', #1357, 1.000000000000000888 ) ;
#15474 = EDGE_CURVE ( 'NONE', #10070, #2702, #952, .T. ) ;
#15475 = CARTESIAN_POINT ( 'NONE',  ( 184.0000000000000568, -181.3058001507315566, -39.95141194869120937 ) ) ;
#15476 = EDGE_CURVE ( 'NONE', #873, #4947, #5623, .T. ) ;
#15477 = ORIENTED_EDGE ( 'NONE', *, *, #10664, .F. ) ;
#15478 = VERTEX_POINT ( 'NONE', #13017 ) ;
#15479 = CYLINDRICAL_SURFACE ( 'NONE', #12722, 3.500000000000003109 ) ;
#15480 = VECTOR ( 'NONE', #14724, 1000.000000000000000 ) ;
#15481 = CARTESIAN_POINT ( 'NONE',  ( 68.56535645333921991, 38.79159067395544014, 5.000000000000000000 ) ) ;
#15482 = LINE ( 'NONE', #3497, #7312 ) ;
#15483 = VERTEX_POINT ( 'NONE', #9337 ) ;
#15484 = CARTESIAN_POINT ( 'NONE',  ( -199.5653198453618700, 142.9393910578133102, -2.963320117457100000 ) ) ;
#15485 = CARTESIAN_POINT ( 'NONE',  ( 209.5531742284681798, 48.05466962632709027, -5.762314779011898480 ) ) ;
#15486 = ORIENTED_EDGE ( 'NONE', *, *, #5460, .T. ) ;
#15487 = ADVANCED_FACE ( 'NONE', ( #11856 ), #4584, .F. ) ;
#15488 = LINE ( 'NONE', #4685, #4779 ) ;
#15489 = DIRECTION ( 'NONE',  ( 0.000000000000000000, 0.000000000000000000, 1.000000000000000000 ) ) ;
#15490 = ADVANCED_FACE ( 'NONE', ( #15304, #4348 ), #943, .T. ) ;
#15491 = CYLINDRICAL_SURFACE ( 'NONE', #7058, 1.000000000000000888 ) ;
#15492 = AXIS2_PLACEMENT_3D ( 'NONE', #4204, #13840, #1839 ) ;
#15493 = ORIENTED_EDGE ( 'NONE', *, *, #218, .T. ) ;
#15494 = CARTESIAN_POINT ( 'NONE',  ( -2.934533493136138205, 18.80010230636893453, -0.3999999999999993006 ) ) ;
#15495 = FILL_AREA_STYLE_COLOUR ( '', #10152 ) ;
#15496 = CARTESIAN_POINT ( 'NONE',  ( 202.9147226314038051, 48.88641379461363101, -0.9068510277452211943 ) ) ;
#15497 = ORIENTED_EDGE ( 'NONE', *, *, #823, .F. ) ;
#15498 = DIRECTION ( 'NONE',  ( 0.000000000000000000, 0.000000000000000000, -1.000000000000000000 ) ) ;
#15499 = CARTESIAN_POINT ( 'NONE',  ( -183.9313806081839289, 121.1548445249323720, 7.918248976830652097 ) ) ;
#15500 = CARTESIAN_POINT ( 'NONE',  ( 0.000000000000000000, 17.53993994372673981, 2.674108611355829274E-15 ) ) ;
#15501 = CARTESIAN_POINT ( 'NONE',  ( 178.0000000000000853, 14.90076684276667862, 37.08491613486885541 ) ) ;
#15502 = CARTESIAN_POINT ( 'NONE',  ( 205.4339596421060889, 33.86846485884471747, -4.932823326473320336 ) ) ;
#15503 = EDGE_CURVE ( 'NONE', #8234, #12311, #9791, .T. ) ;
#15504 = AXIS2_PLACEMENT_3D ( 'NONE', #7451, #14532, #8711 ) ;
#15505 = VERTEX_POINT ( 'NONE', #8003 ) ;
#15506 = EDGE_LOOP ( 'NONE', ( #12379, #2685, #12976 ) ) ;
#15507 = CARTESIAN_POINT ( 'NONE',  ( -223.6145774380523505, 142.0129443944823606, 2.393984899497048513 ) ) ;
#15508 = CARTESIAN_POINT ( 'NONE',  ( 0.01678220609564771287, 0.7854258609844245731, -7.999999999999979572 ) ) ;
#15509 = AXIS2_PLACEMENT_3D ( 'NONE', #15330, #3431, #8263 ) ;
#15510 = DIRECTION ( 'NONE',  ( -1.000000000000000000, 0.000000000000000000, 0.000000000000000000 ) ) ;
#15511 = CARTESIAN_POINT ( 'NONE',  ( 178.0000000000000853, 15.53993994372673804, 37.49999999999991473 ) ) ;
#15512 = CARTESIAN_POINT ( 'NONE',  ( -222.3080144202387203, 148.9395084873732742, -3.019567288340968769 ) ) ;
#15513 = CARTESIAN_POINT ( 'NONE',  ( -218.1626881431459992, 152.3400484335867304, 8.464914971617218953 ) ) ;
#15514 = DIRECTION ( 'NONE',  ( -0.000000000000000000, 0.000000000000000000, 1.000000000000000000 ) ) ;
#15515 = DIRECTION ( 'NONE',  ( 0.000000000000000000, 1.000000000000000000, 0.000000000000000000 ) ) ;
#15516 = CIRCLE ( 'NONE', #9000, 17.06579782980005433 ) ;
#15517 = FACE_OUTER_BOUND ( 'NONE', #15065, .T. ) ;
#15518 = EDGE_CURVE ( 'NONE', #12077, #1137, #5545, .T. ) ;
#15519 = DIRECTION ( 'NONE',  ( -0.000000000000000000, -0.000000000000000000, 1.000000000000000000 ) ) ;
#15520 = CARTESIAN_POINT ( 'NONE',  ( 6.800000000000000711, 0.000000000000000000, -5.400000000000019007 ) ) ;
#15521 = EDGE_LOOP ( 'NONE', ( #2933, #2564 ) ) ;
#15522 = ORIENTED_EDGE ( 'NONE', *, *, #6824, .F. ) ;
#15523 = LINE ( 'NONE', #4808, #8552 ) ;
#15524 = CARTESIAN_POINT ( 'NONE',  ( -70.00000000000000000, 15.53993994372673626, 45.99999999999998579 ) ) ;
#15525 = CARTESIAN_POINT ( 'NONE',  ( 0.000000000000000000, -2.775557561562891351E-14, -8.000000000000007105 ) ) ;
#15526 = DIRECTION ( 'NONE',  ( 0.000000000000000000, -0.000000000000000000, -1.000000000000000000 ) ) ;
#15527 = DIRECTION ( 'NONE',  ( 0.000000000000000000, 0.000000000000000000, -1.000000000000000000 ) ) ;
#15528 = ORIENTED_EDGE ( 'NONE', *, *, #8741, .T. ) ;
#15529 = ORIENTED_EDGE ( 'NONE', *, *, #7018, .F. ) ;
#15530 = CARTESIAN_POINT ( 'NONE',  ( 194.8602319459051557, 33.82038799488785230, -7.127215995405879134 ) ) ;
#15531 = DIRECTION ( 'NONE',  ( 0.000000000000000000, 0.1391731009600591096, -0.9902680687415711391 ) ) ;
#15532 = ORIENTED_EDGE ( 'NONE', *, *, #3820, .T. ) ;
#15533 = FACE_BOUND ( 'NONE', #8078, .T. ) ;
#15534 = CARTESIAN_POINT ( 'NONE',  ( -223.8367800313764064, 146.2004849192998961, 6.377934699871589785 ) ) ;
#15535 = EDGE_LOOP ( 'NONE', ( #5015, #10033, #7063, #848 ) ) ;
#15536 = ORIENTED_EDGE ( 'NONE', *, *, #13204, .F. ) ;
#15537 = DIRECTION ( 'NONE',  ( -0.000000000000000000, 1.000000000000000000, -0.000000000000000000 ) ) ;
#15538 = DIRECTION ( 'NONE',  ( 3.965082230804130220E-16, 4.956352788505162775E-17, -1.000000000000000000 ) ) ;
#15539 = ORIENTED_EDGE ( 'NONE', *, *, #9049, .T. ) ;
#15540 = CARTESIAN_POINT ( 'NONE',  ( -34.79899788034579444, 48.72489408690345414, 10.00000000000000178 ) ) ;
#15541 = ADVANCED_FACE ( 'NONE', ( #11704 ), #11847, .F. ) ;
#15542 = B_SPLINE_CURVE_WITH_KNOTS ( 'NONE', 3,
 ( #10916, #12310, #14677, #8542, #1413, #10989, #8855, #6177, #13333, #3797, #9885, #1261, #14597, #12234, #11062, #6249, #212, #3875, #8699, #12161, #2852, #7675, #14520, #6097, #5214, #13489, #13564, #12390, #1493, #8619, #2773, #4983, #5060, #71, #4910, #3713, #2535, #6331, #7365, #9799, #11143, #298, #5137, #7595 ),
 .UNSPECIFIED., .F., .F.,
 ( 4, 2, 2, 2, 2, 2, 2, 2, 2, 2, 2, 2, 2, 2, 2, 2, 2, 2, 2, 2, 2, 4 ),
 ( 0.000000000000000000, 0.01154246058414762008, 0.06319472280952896648, 0.1156547325041140800, 0.1678637871092111822, 0.2189476930995808979, 0.2714221776790743945, 0.3227197530690046334, 0.3747274728241424824, 0.4267432521036158555, 0.4780248536244998681, 0.5305055628088307662, 0.5815973485975094448, 0.6337991395759137170, 0.6855599279679012170, 0.7371634071600560167, 0.7894711232639126663, 0.8405207634104210346, 0.8929453349049019106, 0.9452650328228678900, 0.9965476795071586125, 1.000000000000000000 ),
 .UNSPECIFIED. ) ;
#15543 = DIRECTION ( 'NONE',  ( 0.000000000000000000, 0.000000000000000000, -1.000000000000000000 ) ) ;
#15544 = ORIENTED_EDGE ( 'NONE', *, *, #8964, .T. ) ;
#15545 = B_SPLINE_CURVE_WITH_KNOTS ( 'NONE', 3,
 ( #15006, #14849, #10286, #1831, #12794, #1982, #13748, #637 ),
 .UNSPECIFIED., .F., .F.,
 ( 4, 2, 2, 4 ),
 ( 0.004673709593152217297, 0.005837709341827692841, 0.007001709090503169253, 0.009329708587854122076 ),
 .UNSPECIFIED. ) ;
#15546 = EDGE_LOOP ( 'NONE', ( #1186, #10065, #14704, #15443 ) ) ;
#15547 =( LENGTH_UNIT ( ) NAMED_UNIT ( * ) SI_UNIT ( .MILLI., .METRE. ) );
#15548 = DIRECTION ( 'NONE',  ( 0.000000000000000000, 0.000000000000000000, -1.000000000000000000 ) ) ;
#15549 = DIRECTION ( 'NONE',  ( -0.000000000000000000, -0.000000000000000000, -1.000000000000000000 ) ) ;
#15550 = ADVANCED_FACE ( 'NONE', ( #10512 ), #12870, .F. ) ;
#15551 = AXIS2_PLACEMENT_3D ( 'NONE', #4512, #9344, #14140 ) ;
#15552 = CARTESIAN_POINT ( 'NONE',  ( -193.7200834347810599, 142.0619459586758921, 2.500000000000000000 ) ) ;
#15553 = DIRECTION ( 'NONE',  ( 0.000000000000000000, 1.000000000000000000, 0.000000000000000000 ) ) ;
#15554 = ORIENTED_EDGE ( 'NONE', *, *, #4830, .F. ) ;
#15555 = EDGE_LOOP ( 'NONE', ( #14848, #10136, #3865, #862 ) ) ;
#15556 = CARTESIAN_POINT ( 'NONE',  ( -194.7245433579248868, 140.1837011942588447, -2.963320117457102665 ) ) ;
#15557 = CARTESIAN_POINT ( 'NONE',  ( 194.8335778941103626, 33.83376941343732369, -4.128887708184892702 ) ) ;
#15558 = AXIS2_PLACEMENT_3D ( 'NONE', #12323, #13815, #11156 ) ;
#15559 = ORIENTED_EDGE ( 'NONE', *, *, #10533, .T. ) ;
#15560 = DIRECTION ( 'NONE',  ( -0.000000000000000000, -1.000000000000000000, -0.000000000000000000 ) ) ;
#15561 = CYLINDRICAL_SURFACE ( 'NONE', #6974, 1.000000000000000888 ) ;
#15562 = DIRECTION ( 'NONE',  ( -0.000000000000000000, -4.956352788505162775E-17, 1.000000000000000000 ) ) ;
#15563 = CIRCLE ( 'NONE', #6014, 6.299128011492294732 ) ;
#15564 = ORIENTED_EDGE ( 'NONE', *, *, #8384, .F. ) ;
#15565 = AXIS2_PLACEMENT_3D ( 'NONE', #14879, #4222, #2905 ) ;
#15566 = APPLICATION_PROTOCOL_DEFINITION ( 'draft international standard', 'automotive_design', 1998, #7496 ) ;
#15567 =( NAMED_UNIT ( * ) PLANE_ANGLE_UNIT ( ) SI_UNIT ( $, .RADIAN. ) );
#15568 = CARTESIAN_POINT ( 'NONE',  ( 201.3910773252651438, 49.55986643532389735, -5.240523689774838623 ) ) ;
#15569 = EDGE_LOOP ( 'NONE', ( #8830, #1177, #4842, #2536, #3156 ) ) ;
#15570 = DIRECTION ( 'NONE',  ( 0.5602235199536450549, 0.8138631617988982825, 0.1541958545404128744 ) ) ;
#15571 = DIRECTION ( 'NONE',  ( -0.000000000000000000, 1.000000000000000000, -0.000000000000000000 ) ) ;
#15572 = EDGE_CURVE ( 'NONE', #2689, #12589, #9541, .T. ) ;
#15573 = CARTESIAN_POINT ( 'NONE',  ( -194.2694872093395873, 127.5478817636406035, 5.434137442415935659 ) ) ;
#15576 = ADVANCED_FACE ( 'NONE', ( #8241 ), #10440, .F. ) ;
#15575 = EDGE_CURVE ( 'NONE', #14187, #8873, #14310, .T. ) ;
#15574 = CARTESIAN_POINT ( 'NONE',  ( -76.50000000000001421, 15.10952649420676686, 25.44255979523916977 ) ) ;
#15577 = ORIENTED_EDGE ( 'NONE', *, *, #13835, .F. ) ;
#15578 = CARTESIAN_POINT ( 'NONE',  ( -207.1471226269450767, 137.0919095985319132, 9.577123744044238052 ) ) ;
#15579 = FACE_OUTER_BOUND ( 'NONE', #4942, .T. ) ;
#15580 = VECTOR ( 'NONE', #6096, 1000.000000000000000 ) ;
#15581 = ORIENTED_EDGE ( 'NONE', *, *, #5761, .T. ) ;
#15582 = ORIENTED_EDGE ( 'NONE', *, *, #6390, .T. ) ;
#15583 = CARTESIAN_POINT ( 'NONE',  ( -33.09899788034579871, 48.72489408690345414, 10.00000000000000178 ) ) ;
#15584 = FACE_OUTER_BOUND ( 'NONE', #6031, .T. ) ;
#15585 = AXIS2_PLACEMENT_3D ( 'NONE', #5221, #9973, #9514 ) ;
#15586 = CIRCLE ( 'NONE', #7798, 20.41351791792154913 ) ;
#15587 = CARTESIAN_POINT ( 'NONE',  ( -76.50000000000004263, 15.17911304468679745, 25.93769382960994818 ) ) ;
#15588 = CARTESIAN_POINT ( 'NONE',  ( 200.1062858801516597, 40.86394065090267702, 5.000000000000000000 ) ) ;
#15589 = LINE ( 'NONE', #39, #13876 ) ;
#15590 = CARTESIAN_POINT ( 'NONE',  ( -220.9230348769640102, 147.2864796216551326, 9.830311889130468828 ) ) ;
#15591 = CARTESIAN_POINT ( 'NONE',  ( 171.7208925888976978, 62.57671370024034729, -0.9107274384406883749 ) ) ;
#15592 = VECTOR ( 'NONE', #8541, 1000.000000000000000 ) ;
#15593 = DIRECTION ( 'NONE',  ( 1.000000000000000000, 0.000000000000000000, 0.000000000000000000 ) ) ;
#15594 = CARTESIAN_POINT ( 'NONE',  ( -63.50000000000002842, 17.53993994372673981, -17.50000000000002487 ) ) ;
#15595 = VECTOR ( 'NONE', #5945, 1000.000000000000000 ) ;
#15596 = DIRECTION ( 'NONE',  ( 0.000000000000000000, 0.000000000000000000, 1.000000000000000000 ) ) ;
#15597 = CARTESIAN_POINT ( 'NONE',  ( 184.0000000000000568, 17.53993994372673271, 48.99999999999997158 ) ) ;
#15598 = ORIENTED_EDGE ( 'NONE', *, *, #11840, .T. ) ;
#15599 = ORIENTED_EDGE ( 'NONE', *, *, #11356, .T. ) ;
#15600 = CARTESIAN_POINT ( 'NONE',  ( 200.1062858801516597, 40.86394065090267702, 18.00000000000000355 ) ) ;
#15601 = DIRECTION ( 'NONE',  ( 0.000000000000000000, 0.7071067811865474617, 0.7071067811865474617 ) ) ;
#15602 = CIRCLE ( 'NONE', #9085, 1.000000000000000888 ) ;
#15603 = DIRECTION ( 'NONE',  ( 0.000000000000000000, 1.000000000000000000, 0.000000000000000000 ) ) ;
#15604 = ADVANCED_FACE ( 'NONE', ( #2215 ), #12966, .T. ) ;
#15605 = VECTOR ( 'NONE', #10776, 1000.000000000000000 ) ;
#15606 =( NAMED_UNIT ( * ) PLANE_ANGLE_UNIT ( ) SI_UNIT ( $, .RADIAN. ) );
#15607 = PLANE ( 'NONE',  #14273 ) ;
#15608 = CIRCLE ( 'NONE', #15109, 6.999999999999978684 ) ;
#15609 = LINE ( 'NONE', #8460, #3531 ) ;
#15610 = DIRECTION ( 'NONE',  ( 0.000000000000000000, 0.000000000000000000, -1.000000000000000000 ) ) ;
#15611 = APPLICATION_CONTEXT ( 'automotive_design' ) ;
#15612 = ORIENTED_EDGE ( 'NONE', *, *, #1988, .F. ) ;
#15613 = ADVANCED_FACE ( 'NONE', ( #11605 ), #768, .F. ) ;
#15614 = AXIS2_PLACEMENT_3D ( 'NONE', #15264, #14246, #3290 ) ;
#15615 = VECTOR ( 'NONE', #7189, 1000.000000000000000 ) ;
#15616 = ADVANCED_BREP_SHAPE_REPRESENTATION ( '', ( #243, #12337 ), #10810 ) ;
#15617 = ORIENTED_EDGE ( 'NONE', *, *, #8880, .T. ) ;
#15618 = DIRECTION ( 'NONE',  ( 0.000000000000000000, 1.000000000000000000, 0.000000000000000000 ) ) ;
#15619 = NEXT_ASSEMBLY_USAGE_OCCURRENCE ( 'NAUO1', ' ', ' ', #14036, #12586, $ ) ;
#15620 = NEXT_ASSEMBLY_USAGE_OCCURRENCE ( 'NAUO2', ' ', ' ', #14036, #15380, $ ) ;
#15621 = NEXT_ASSEMBLY_USAGE_OCCURRENCE ( 'NAUO3', ' ', ' ', #14036, #4976, $ ) ;
#15622 = NEXT_ASSEMBLY_USAGE_OCCURRENCE ( 'NAUO4', ' ', ' ', #14036, #10574, $ ) ;
#15623 = NEXT_ASSEMBLY_USAGE_OCCURRENCE ( 'NAUO5', ' ', ' ', #14036, #6143, $ ) ;
#15624 = NEXT_ASSEMBLY_USAGE_OCCURRENCE ( 'NAUO6', ' ', ' ', #14036, #8944, $ ) ;
#15625 = NEXT_ASSEMBLY_USAGE_OCCURRENCE ( 'NAUO7', ' ', ' ', #14036, #6635, $ ) ;
#15626 = NEXT_ASSEMBLY_USAGE_OCCURRENCE ( 'NAUO8', ' ', ' ', #14036, #14513, $ ) ;
#15627 = NEXT_ASSEMBLY_USAGE_OCCURRENCE ( 'NAUO9', ' ', ' ', #14036, #12882, $ ) ;
#15628 = NEXT_ASSEMBLY_USAGE_OCCURRENCE ( 'NAUO10', ' ', ' ', #14036, #12882, $ ) ;
#15629 = NEXT_ASSEMBLY_USAGE_OCCURRENCE ( 'NAUO11', ' ', ' ', #14036, #12882, $ ) ;
#15630 = NEXT_ASSEMBLY_USAGE_OCCURRENCE ( 'NAUO12', ' ', ' ', #14036, #12882, $ ) ;
#15631 = NEXT_ASSEMBLY_USAGE_OCCURRENCE ( 'NAUO13', ' ', ' ', #14036, #12882, $ ) ;
#15632 = NEXT_ASSEMBLY_USAGE_OCCURRENCE ( 'NAUO14', ' ', ' ', #14036, #12882, $ ) ;
#15633 = NEXT_ASSEMBLY_USAGE_OCCURRENCE ( 'NAUO15', ' ', ' ', #14036, #5848, $ ) ;
ENDSEC;
END-ISO-10303-21;
